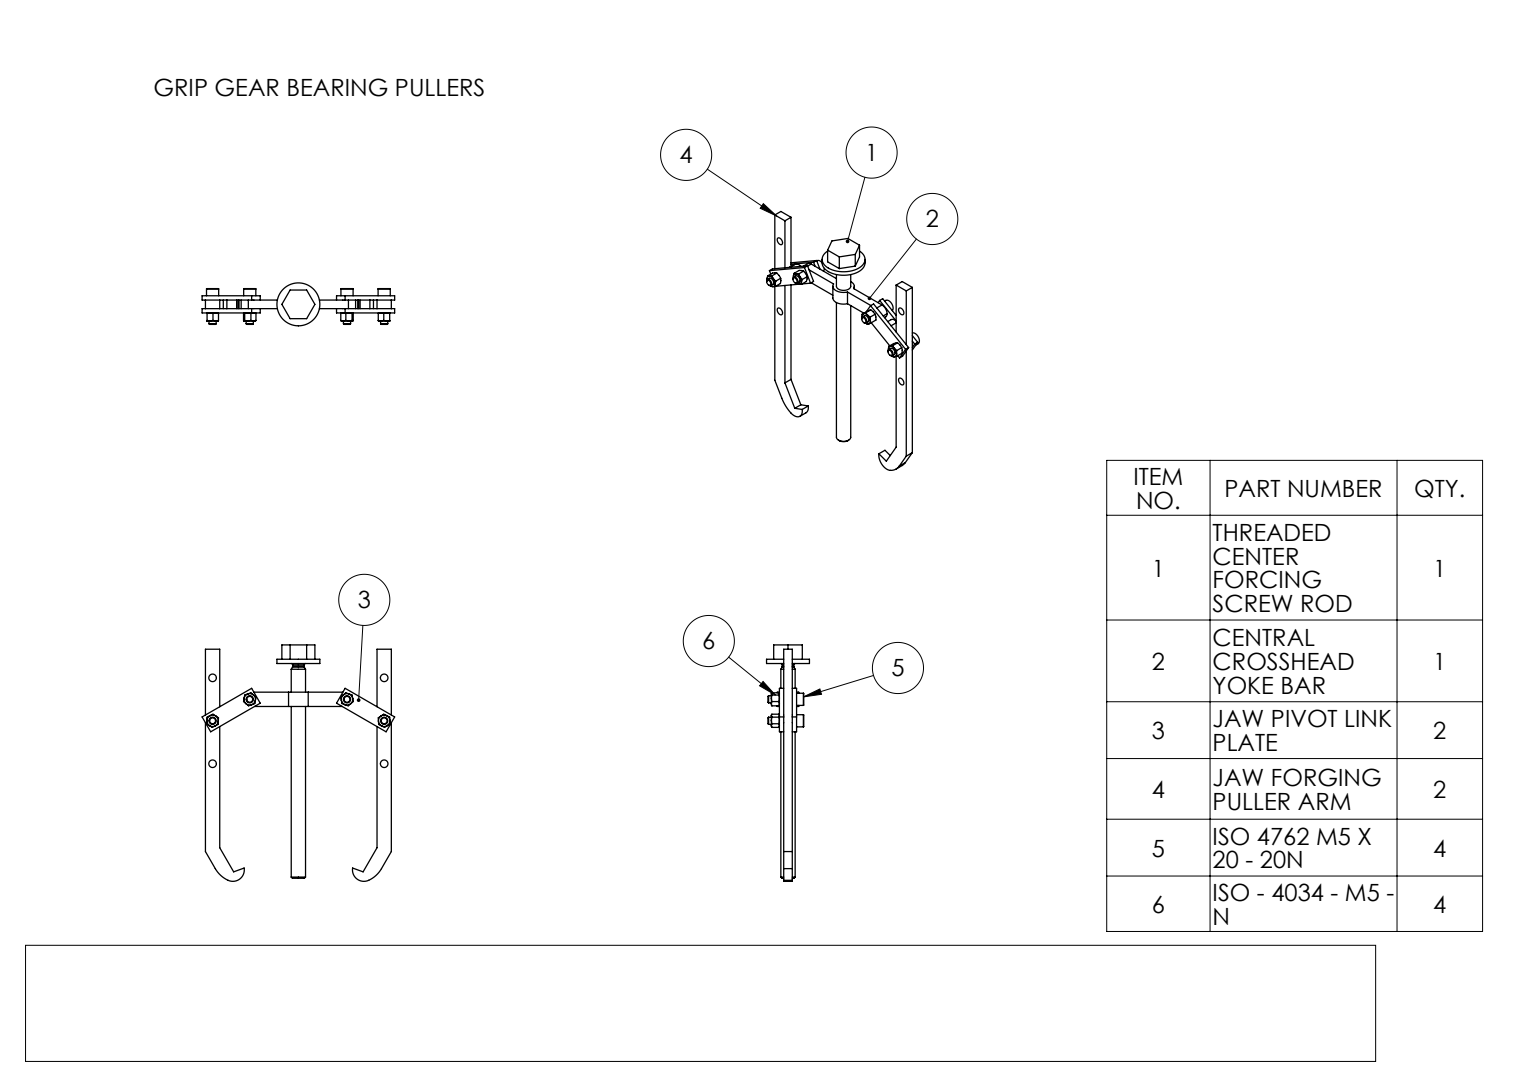
ISO-10303-21;
HEADER;
FILE_DESCRIPTION (('STEP AP214'),
    '1' );
FILE_NAME ('MAS-182',
    '2026-10-22T13:24:12',
    ( '' ),
    ( '' ),
    'SwSTEP 2.0',
    'SolidWorks 2026',
    '' );
FILE_SCHEMA (( 'AUTOMOTIVE_DESIGN' ));
ENDSEC;

DATA;
#1 = DIRECTION ( 'NONE',  ( 1.000000000000000000, 0.000000000000000000, 0.000000000000000000 ) ) ;
#2 = CARTESIAN_POINT ( 'NONE',  ( 0.000000000000000000, -150.0000000000000000, 0.000000000000000000 ) ) ;
#3 = AXIS2_PLACEMENT_3D ( 'NONE', #2223, #202, #1998 ) ;
#4 = EDGE_CURVE ( 'NONE', #2839, #391, #2268, .T. ) ;
#5 = LINE ( 'NONE', #437, #2768 ) ;
#6 = VECTOR ( 'NONE', #2626, 1000.000000000000114 ) ;
#7 = VECTOR ( 'NONE', #1963, 1000.000000000000000 ) ;
#8 = ORIENTED_EDGE ( 'NONE', *, *, #1854, .F. ) ;
#9 = CARTESIAN_POINT ( 'NONE',  ( -18.00961894323348389, -42.69615242270662492, -3.000000000000000000 ) ) ;
#10 = PLANE ( 'NONE',  #689 ) ;
#11 = AXIS2_PLACEMENT_3D ( 'NONE', #480, #2053, #1136 ) ;
#12 = CARTESIAN_POINT ( 'NONE',  ( 5.510910596163087583E-16, -0.9999999999999997780, -3.999999999999999112 ) ) ;
#13 = COLOUR_RGB ( '',0.8941176470588234615, 0.8941176470588234615, 0.8941176470588234615 ) ;
#14 = DIRECTION ( 'NONE',  ( -1.000000000000000000, 0.000000000000000000, 1.502314598737159524E-16 ) ) ;
#15 = VERTEX_POINT ( 'NONE', #913 ) ;
#16 = DIRECTION ( 'NONE',  ( 0.000000000000000000, 0.000000000000000000, -1.000000000000000000 ) ) ;
#17 = DIRECTION ( 'NONE',  ( -1.000000000000000000, 0.000000000000000000, 3.004629197474320528E-16 ) ) ;
#18 = DIRECTION ( 'NONE',  ( -0.000000000000000000, -1.000000000000000000, -0.000000000000000000 ) ) ;
#19 = VECTOR ( 'NONE', #1794, 1000.000000000000000 ) ;
#20 = PRODUCT_DEFINITION_SHAPE ( 'NONE', 'NONE',  #1387 ) ;
#21 = EDGE_CURVE ( 'NONE', #1828, #1252, #472, .T. ) ;
#22 = VECTOR ( 'NONE', #2319, 1000.000000000000000 ) ;
#23 = VERTEX_POINT ( 'NONE', #2540 ) ;
#24 = DIRECTION ( 'NONE',  ( 0.000000000000000000, 0.7071067811865452413, 0.7071067811865497932 ) ) ;
#25 = FACE_OUTER_BOUND ( 'NONE', #1470, .T. ) ;
#26 = VERTEX_POINT ( 'NONE', #2286 ) ;
#27 = CARTESIAN_POINT ( 'NONE',  ( -5.773502691896258199, 13.00000000000000178, -9.999999999999998224 ) ) ;
#28 = EDGE_CURVE ( 'NONE', #2653, #1371, #1839, .T. ) ;
#29 = ORIENTED_EDGE ( 'NONE', *, *, #1848, .F. ) ;
#30 = DIRECTION ( 'NONE',  ( -1.000000000000000000, 0.000000000000000000, 0.000000000000000000 ) ) ;
#31 = FACE_OUTER_BOUND ( 'NONE', #195, .T. ) ;
#32 = FACE_OUTER_BOUND ( 'NONE', #973, .T. ) ;
#33 = CARTESIAN_POINT ( 'NONE',  ( -32.66987298107778059, -17.30384757729337508, 6.000000000000000000 ) ) ;
#34 = ORIENTED_EDGE ( 'NONE', *, *, #947, .F. ) ;
#35 = DIRECTION ( 'NONE',  ( 1.000000000000000000, 0.000000000000000000, 0.000000000000000000 ) ) ;
#36 = EDGE_CURVE ( 'NONE', #1503, #53, #2280, .T. ) ;
#37 = CARTESIAN_POINT ( 'NONE',  ( -36.64999999999999147, -25.00000000000000000, 6.000000000000000888 ) ) ;
#38 = ADVANCED_FACE ( 'NONE', ( #500, #1172 ), #2089, .T. ) ;
#39 = DIRECTION ( 'NONE',  ( -1.000000000000000000, 0.000000000000000000, 0.000000000000000000 ) ) ;
#40 = SURFACE_SIDE_STYLE ('',( #2060 ) ) ;
#41 = ORIENTED_EDGE ( 'NONE', *, *, #2625, .F. ) ;
#42 = CARTESIAN_POINT ( 'NONE',  ( -43.16025403784440329, -29.13397459621553764, 3.000000000000002220 ) ) ;
#43 = DIRECTION ( 'NONE',  ( -0.000000000000000000, -1.000000000000000000, -0.000000000000000000 ) ) ;
#44 = DIRECTION ( 'NONE',  ( 0.000000000000000000, 1.000000000000000000, 0.000000000000000000 ) ) ;
#45 = FACE_OUTER_BOUND ( 'NONE', #672, .T. ) ;
#46 = AXIS2_PLACEMENT_3D ( 'NONE', #1452, #789, #2135 ) ;
#47 = EDGE_LOOP ( 'NONE', ( #341, #1054, #52, #1581 ) ) ;
#48 = CARTESIAN_POINT ( 'NONE',  ( -34.99999999999999289, -20.00000000000000000, 3.000000000000000000 ) ) ;
#49 = CIRCLE ( 'NONE', #831, 7.500000000000000888 ) ;
#50 = FACE_BOUND ( 'NONE', #2831, .T. ) ;
#51 = AXIS2_PLACEMENT_3D ( 'NONE', #933, #1833, #2774 ) ;
#52 = ORIENTED_EDGE ( 'NONE', *, *, #1034, .T. ) ;
#53 = VERTEX_POINT ( 'NONE', #12 ) ;
#54 = AXIS2_PLACEMENT_3D ( 'NONE', #2910, #888, #418 ) ;
#55 = EDGE_CURVE ( 'NONE', #2070, #608, #62, .T. ) ;
#56 = CARTESIAN_POINT ( 'NONE',  ( 0.000000000000000000, -1.000000000000000000, 0.000000000000000000 ) ) ;
#57 = ORIENTED_EDGE ( 'NONE', *, *, #910, .F. ) ;
#58 = AXIS2_PLACEMENT_3D ( 'NONE', #1165, #883, #1343 ) ;
#59 = CARTESIAN_POINT ( 'NONE',  ( -58.09974666316955449, -143.2580143298517328, -3.000000000000000000 ) ) ;
#60 = DIRECTION ( 'NONE',  ( -0.8660254037844401509, -0.4999999999999971689, 1.469576158976821827E-16 ) ) ;
#61 = DIRECTION ( 'NONE',  ( 1.000000000000000000, 0.000000000000000000, 0.000000000000000000 ) ) ;
#62 = CIRCLE ( 'NONE', #204, 20.00000000000000355 ) ;
#63 = AXIS2_PLACEMENT_3D ( 'NONE', #554, #2133, #1693 ) ;
#64 = ORIENTED_EDGE ( 'NONE', *, *, #1925, .F. ) ;
#65 = EDGE_CURVE ( 'NONE', #415, #110, #2593, .T. ) ;
#66 = PLANE ( 'NONE',  #2475 ) ;
#67 = AXIS2_PLACEMENT_3D ( 'NONE', #278, #535, #1657 ) ;
#68 = EDGE_CURVE ( 'NONE', #2151, #2048, #2812, .T. ) ;
#69 = LINE ( 'NONE', #303, #372 ) ;
#70 = ORIENTED_EDGE ( 'NONE', *, *, #879, .F. ) ;
#71 = CIRCLE ( 'NONE', #1705, 4.999999999999998224 ) ;
#72 = CARTESIAN_POINT ( 'NONE',  ( -52.65063509461111835, -62.69615242270656807, -3.000000000000000000 ) ) ;
#73 = CARTESIAN_POINT ( 'NONE',  ( -43.99038105676666532, -37.69615242270662492, 3.000000000000002665 ) ) ;
#74 = ORIENTED_EDGE ( 'NONE', *, *, #1121, .T. ) ;
#75 = EDGE_CURVE ( 'NONE', #120, #1771, #154, .T. ) ;
#76 = CYLINDRICAL_SURFACE ( 'NONE', #302, 2.649999999999985700 ) ;
#77 = FILL_AREA_STYLE_COLOUR ( '', #559 ) ;
#78 = LINE ( 'NONE', #2340, #2456 ) ;
#79 = FACE_BOUND ( 'NONE', #2327, .T. ) ;
#80 = EDGE_CURVE ( 'NONE', #1900, #237, #994, .T. ) ;
#81 = VERTEX_POINT ( 'NONE', #86 ) ;
#82 = LINE ( 'NONE', #1419, #2817 ) ;
#83 = VERTEX_POINT ( 'NONE', #98 ) ;
#84 = CARTESIAN_POINT ( 'NONE',  ( -39.99999999999999289, -30.00000000000000000, -3.000000000000000000 ) ) ;
#85 = ORIENTED_EDGE ( 'NONE', *, *, #1055, .F. ) ;
#86 = CARTESIAN_POINT ( 'NONE',  ( 0.000000000000000000, -149.1719999999999970, 5.000000000000000000 ) ) ;
#87 = CARTESIAN_POINT ( 'NONE',  ( -59.98076211353318854, -39.99999999999994316, 6.000000000000000888 ) ) ;
#88 = ORIENTED_EDGE ( 'NONE', *, *, #2477, .T. ) ;
#89 = LINE ( 'NONE', #2576, #346 ) ;
#90 = DIRECTION ( 'NONE',  ( 0.8660254037844383745, 0.000000000000000000, -0.5000000000000004441 ) ) ;
#91 = DIRECTION ( 'NONE',  ( -0.000000000000000000, -0.000000000000000000, 1.000000000000000000 ) ) ;
#92 = EDGE_CURVE ( 'NONE', #1675, #1139, #1237, .T. ) ;
#93 = VERTEX_POINT ( 'NONE', #2360 ) ;
#94 = AXIS2_PLACEMENT_3D ( 'NONE', #273, #1403, #2068 ) ;
#95 = PLANE ( 'NONE',  #2598 ) ;
#96 = EDGE_LOOP ( 'NONE', ( #402, #361, #2058, #215 ) ) ;
#97=STYLED_ITEM('',(#2949),#2534);
#98 = CARTESIAN_POINT ( 'NONE',  ( -62.63076211353318712, -9.999999999999943157, 3.000000000000001332 ) ) ;
#99 = CARTESIAN_POINT ( 'NONE',  ( -31.35000000000001563, -25.00000000000000000, -3.000000000000001332 ) ) ;
#100 = EDGE_LOOP ( 'NONE', ( #2045, #2281 ) ) ;
#101 = MECHANICAL_DESIGN_GEOMETRIC_PRESENTATION_REPRESENTATION (  '', ( #833 ), #2032 ) ;
#102 = DIRECTION ( 'NONE',  ( -1.000000000000000000, 0.000000000000000000, 0.000000000000000000 ) ) ;
#103 = VECTOR ( 'NONE', #2064, 1000.000000000000114 ) ;
#104 = FILL_AREA_STYLE ('',( #77 ) ) ;
#105 = CARTESIAN_POINT ( 'NONE',  ( -31.00000000000002132, -30.19615242270664268, -3.000000000000000888 ) ) ;
#106 = ADVANCED_FACE ( 'NONE', ( #985 ), #566, .F. ) ;
#107 = VECTOR ( 'NONE', #1157, 1000.000000000000000 ) ;
#108 = ORIENTED_EDGE ( 'NONE', *, *, #1186, .F. ) ;
#109 = CLOSED_SHELL ( 'NONE', ( #2797, #1837, #1415, #550, #392, #827, #441, #1532, #2192, #615, #2313, #2289, #2566, #2325, #660, #1443, #890 ) ) ;
#110 = VERTEX_POINT ( 'NONE', #332 ) ;
#111 = EDGE_CURVE ( 'NONE', #2201, #2834, #2628, .T. ) ;
#112 = VECTOR ( 'NONE', #2880, 1000.000000000000000 ) ;
#113 = EDGE_CURVE ( 'NONE', #132, #2201, #803, .T. ) ;
#114 = LINE ( 'NONE', #1010, #6 ) ;
#115 = EDGE_LOOP ( 'NONE', ( #29, #1418, #842, #2140 ) ) ;
#116 = DIRECTION ( 'NONE',  ( 1.000000000000000000, 0.000000000000000000, 0.000000000000000000 ) ) ;
#117 = AXIS2_PLACEMENT_3D ( 'NONE', #1191, #1902, #2801 ) ;
#118 = DIRECTION ( 'NONE',  ( 0.000000000000000000, 0.000000000000000000, 1.000000000000000000 ) ) ;
#119 = CIRCLE ( 'NONE', #1751, 4.999999999999997335 ) ;
#120 = VERTEX_POINT ( 'NONE', #127 ) ;
#121 = SURFACE_STYLE_USAGE ( .BOTH. , #1056 ) ;
#122 = LINE ( 'NONE', #1519, #2601 ) ;
#123 = ORIENTED_EDGE ( 'NONE', *, *, #92, .F. ) ;
#124 = PRESENTATION_STYLE_ASSIGNMENT (( #2199 ) ) ;
#125 = ORIENTED_EDGE ( 'NONE', *, *, #2038, .F. ) ;
#126 = DIRECTION ( 'NONE',  ( -0.8660254037844390407, 0.000000000000000000, -0.4999999999999993339 ) ) ;
#127 = CARTESIAN_POINT ( 'NONE',  ( -37.91455138073065001, -142.8479302707733041, -3.000000000000000000 ) ) ;
#128 = CARTESIAN_POINT ( 'NONE',  ( -62.63076211353317291, -39.99999999999994316, -3.000000000000005329 ) ) ;
#129 = EDGE_CURVE ( 'NONE', #732, #608, #1011, .T. ) ;
#130 = ORIENTED_EDGE ( 'NONE', *, *, #1665, .T. ) ;
#131 = DIRECTION ( 'NONE',  ( -0.000000000000000000, -0.000000000000000000, 1.000000000000000000 ) ) ;
#132 = VERTEX_POINT ( 'NONE', #1872 ) ;
#133 = DIRECTION ( 'NONE',  ( -2.312964634635742661E-15, 0.000000000000000000, -1.000000000000000000 ) ) ;
#134 =( NAMED_UNIT ( * ) PLANE_ANGLE_UNIT ( ) SI_UNIT ( $, .RADIAN. ) );
#135 = ORIENTED_EDGE ( 'NONE', *, *, #1188, .F. ) ;
#136 = DIRECTION ( 'NONE',  ( 0.000000000000000000, 0.000000000000000000, 1.000000000000000000 ) ) ;
#137 = DIRECTION ( 'NONE',  ( 0.000000000000000000, 0.000000000000000000, 1.000000000000000000 ) ) ;
#138 = SHAPE_DEFINITION_REPRESENTATION ( #683, #470 ) ;
#139 = DIRECTION ( 'NONE',  ( -1.000000000000000000, 0.000000000000000000, 1.272690286469888396E-16 ) ) ;
#140 = EDGE_LOOP ( 'NONE', ( #2113, #808, #665, #2884, #381 ) ) ;
#141 = AXIS2_PLACEMENT_3D ( 'NONE', #801, #2592, #136 ) ;
#142 = EDGE_CURVE ( 'NONE', #1729, #1249, #2519, .T. ) ;
#143 = CARTESIAN_POINT ( 'NONE',  ( -57.33076211353320417, -69.99999999999995737, 3.000000000000001332 ) ) ;
#144 = DIRECTION ( 'NONE',  ( 1.000000000000000000, 0.000000000000000000, -2.341876692568690761E-15 ) ) ;
#145 = TOROIDAL_SURFACE ( 'NONE', #1548, 4.999999999999998224, 0.9999999999999995559 ) ;
#146 = ORIENTED_EDGE ( 'NONE', *, *, #1085, .T. ) ;
#147 = CYLINDRICAL_SURFACE ( 'NONE', #663, 5.000000000000000888 ) ;
#148=STYLED_ITEM('',(#2977),#1527);
#149 = ORIENTED_EDGE ( 'NONE', *, *, #1965, .T. ) ;
#150 = CIRCLE ( 'NONE', #652, 2.649999999999985700 ) ;
#151 = CARTESIAN_POINT ( 'NONE',  ( -31.00000000000002132, -30.19615242270664268, 6.000000000000000000 ) ) ;
#152 = EDGE_CURVE ( 'NONE', #1771, #732, #1431, .T. ) ;
#153 = CYLINDRICAL_SURFACE ( 'NONE', #1179, 3.999999999999998224 ) ;
#154 = CIRCLE ( 'NONE', #1792, 8.000000000000000000 ) ;
#155 = APPLICATION_PROTOCOL_DEFINITION ( 'draft international standard', 'automotive_design', 1998, #2613 ) ;
#156 = CARTESIAN_POINT ( 'NONE',  ( -18.00961894323348389, -42.69615242270662492, 3.000000000000000000 ) ) ;
#157 = EDGE_LOOP ( 'NONE', ( #1667, #2865, #926, #590, #162 ) ) ;
#158 = VECTOR ( 'NONE', #1568, 1000.000000000000000 ) ;
#159 = SURFACE_STYLE_FILL_AREA ( #1906 ) ;
#160 = DIRECTION ( 'NONE',  ( 1.000000000000000000, 0.000000000000000000, 0.000000000000000000 ) ) ;
#161 = ADVANCED_FACE ( 'NONE', ( #1024 ), #786, .F. ) ;
#162 = ORIENTED_EDGE ( 'NONE', *, *, #1048, .T. ) ;
#163 = FACE_OUTER_BOUND ( 'NONE', #394, .T. ) ;
#164 = EDGE_CURVE ( 'NONE', #1727, #2749, #1701, .T. ) ;
#165 = EDGE_LOOP ( 'NONE', ( #896, #1637 ) ) ;
#166 =( NAMED_UNIT ( * ) SI_UNIT ( $, .STERADIAN. ) SOLID_ANGLE_UNIT ( ) );
#167 = VERTEX_POINT ( 'NONE', #2852 ) ;
#168 = DIRECTION ( 'NONE',  ( -0.000000000000000000, -0.000000000000000000, 1.000000000000000000 ) ) ;
#169 = CARTESIAN_POINT ( 'NONE',  ( 0.000000000000000000, 0.000000000000000000, 0.000000000000000000 ) ) ;
#170 = CARTESIAN_POINT ( 'NONE',  ( 34.00000000000000000, -25.00000000000000000, -3.000000000000001332 ) ) ;
#171 = ORIENTED_EDGE ( 'NONE', *, *, #2056, .F. ) ;
#172 = CYLINDRICAL_SURFACE ( 'NONE', #2274, 3.999999999999998224 ) ;
#173 = CARTESIAN_POINT ( 'NONE',  ( -46.49038105676660848, -33.36602540378440551, -2.999999999999996891 ) ) ;
#174 = ORIENTED_EDGE ( 'NONE', *, *, #892, .F. ) ;
#175 = DIRECTION ( 'NONE',  ( 1.000000000000000000, 0.000000000000000000, 0.000000000000000000 ) ) ;
#176 = SHAPE_REPRESENTATION ( 'MAS-182', ( #2707, #1310, #743, #936, #2461 ), #1979 ) ;
#177 = ORIENTED_EDGE ( 'NONE', *, *, #2792, .T. ) ;
#178 = ADVANCED_FACE ( 'NONE', ( #1439 ), #582, .T. ) ;
#179 = CARTESIAN_POINT ( 'NONE',  ( -6.873863542433761076, -20.00000000000000000, 3.000000000000000000 ) ) ;
#180 = CYLINDRICAL_SURFACE ( 'NONE', #659, 2.649999999999985700 ) ;
#181 = ORIENTED_EDGE ( 'NONE', *, *, #773, .F. ) ;
#182 =( NAMED_UNIT ( * ) SI_UNIT ( $, .STERADIAN. ) SOLID_ANGLE_UNIT ( ) );
#183 = FACE_OUTER_BOUND ( 'NONE', #2189, .T. ) ;
#184 = ORIENTED_EDGE ( 'NONE', *, *, #1754, .T. ) ;
#185 = CIRCLE ( 'NONE', #2071, 2.649999999999985700 ) ;
#186 = DIRECTION ( 'NONE',  ( 1.000000000000000000, 0.000000000000000000, 0.000000000000000000 ) ) ;
#187 = DIRECTION ( 'NONE',  ( -0.000000000000000000, -1.000000000000000000, -0.000000000000000000 ) ) ;
#188 = EDGE_LOOP ( 'NONE', ( #1239, #2686, #729, #1617 ) ) ;
#189 = AXIS2_PLACEMENT_3D ( 'NONE', #2895, #2216, #1972 ) ;
#190 = LINE ( 'NONE', #904, #997 ) ;
#191 = EDGE_CURVE ( 'NONE', #790, #1718, #2828, .T. ) ;
#192 = DIRECTION ( 'NONE',  ( -1.076523719386531503E-16, -6.215312591768280423E-17, 1.000000000000000000 ) ) ;
#193 = AXIS2_PLACEMENT_3D ( 'NONE', #1698, #1267, #144 ) ;
#194 = DIRECTION ( 'NONE',  ( 1.000000000000000000, 0.000000000000000000, 0.000000000000000000 ) ) ;
#195 = EDGE_LOOP ( 'NONE', ( #2000, #2767, #2469, #1038, #802, #746 ) ) ;
#196 = COLOUR_RGB ( '',0.8941176470588234615, 0.8941176470588234615, 0.8941176470588234615 ) ;
#197 = VECTOR ( 'NONE', #522, 1000.000000000000000 ) ;
#198 = LINE ( 'NONE', #2410, #1162 ) ;
#199 = EDGE_CURVE ( 'NONE', #2240, #2529, #1039, .T. ) ;
#200 = FACE_OUTER_BOUND ( 'NONE', #1652, .T. ) ;
#201 =( LENGTH_UNIT ( ) NAMED_UNIT ( * ) SI_UNIT ( .MILLI., .METRE. ) );
#202 = DIRECTION ( 'NONE',  ( -0.000000000000000000, -0.000000000000000000, 1.000000000000000000 ) ) ;
#203 = ORIENTED_EDGE ( 'NONE', *, *, #1188, .T. ) ;
#204 = AXIS2_PLACEMENT_3D ( 'NONE', #900, #2724, #531 ) ;
#205 = DIRECTION ( 'NONE',  ( -1.000000000000000000, 0.000000000000000000, 1.636531581110204284E-16 ) ) ;
#206 = AXIS2_PLACEMENT_3D ( 'NONE', #1277, #1543, #609 ) ;
#207 = FILL_AREA_STYLE_COLOUR ( '', #2269 ) ;
#208 = EDGE_LOOP ( 'NONE', ( #779, #2624, #1671, #1565 ) ) ;
#209 = DIRECTION ( 'NONE',  ( 0.000000000000000000, 0.000000000000000000, 1.000000000000000000 ) ) ;
#210 = VECTOR ( 'NONE', #2756, 1000.000000000000000 ) ;
#211 = CARTESIAN_POINT ( 'NONE',  ( -59.98076211353318854, -69.99999999999995737, 3.000000000000000000 ) ) ;
#212 = VECTOR ( 'NONE', #1969, 1000.000000000000000 ) ;
#213 = DIRECTION ( 'NONE',  ( -0.000000000000000000, -0.000000000000000000, -1.000000000000000000 ) ) ;
#214 = LINE ( 'NONE', #690, #2553 ) ;
#215 = ORIENTED_EDGE ( 'NONE', *, *, #2027, .T. ) ;
#216 = CARTESIAN_POINT ( 'NONE',  ( -31.35000000000001563, -25.00000000000000000, -3.000000000000001332 ) ) ;
#217 = DIRECTION ( 'NONE',  ( 0.000000000000000000, -0.000000000000000000, 1.000000000000000000 ) ) ;
#218 = VERTEX_POINT ( 'NONE', #1654 ) ;
#219 = EDGE_CURVE ( 'NONE', #1447, #1073, #1678, .T. ) ;
#220 = PLANE ( 'NONE',  #1032 ) ;
#221 = DIRECTION ( 'NONE',  ( 0.000000000000000000, 0.000000000000000000, -1.000000000000000000 ) ) ;
#222 = EDGE_LOOP ( 'NONE', ( #1224, #1858, #149, #2137 ) ) ;
#223 = DIRECTION ( 'NONE',  ( -1.000000000000000000, 0.000000000000000000, 0.000000000000000000 ) ) ;
#224 = CARTESIAN_POINT ( 'NONE',  ( -59.98076211353319565, -9.999999999999943157, 3.000000000000000000 ) ) ;
#225 = DIRECTION ( 'NONE',  ( -0.4999999999999977796, 0.8660254037844399289, 0.000000000000000000 ) ) ;
#226 = ORIENTED_EDGE ( 'NONE', *, *, #1897, .F. ) ;
#227 = CARTESIAN_POINT ( 'NONE',  ( 0.000000000000000000, -30.00000000000000000, 0.000000000000000000 ) ) ;
#228 = DIRECTION ( 'NONE',  ( -0.000000000000000000, -1.000000000000000000, -0.000000000000000000 ) ) ;
#229 = EDGE_LOOP ( 'NONE', ( #1491, #1391 ) ) ;
#230 = CARTESIAN_POINT ( 'NONE',  ( -64.98076211353318854, 10.00000000000005684, -3.000000000000000000 ) ) ;
#231 = CARTESIAN_POINT ( 'NONE',  ( 0.000000000000000000, 0.000000000000000000, 0.000000000000000000 ) ) ;
#232 = ORIENTED_EDGE ( 'NONE', *, *, #2574, .F. ) ;
#233 = EDGE_CURVE ( 'NONE', #1447, #2315, #1733, .T. ) ;
#234 = CARTESIAN_POINT ( 'NONE',  ( -59.98076211353318854, -39.99999999999994316, 3.000000000000000444 ) ) ;
#235 = DIRECTION ( 'NONE',  ( -1.000000000000000000, 0.000000000000000000, -0.000000000000000000 ) ) ;
#236 = VECTOR ( 'NONE', #2191, 1000.000000000000000 ) ;
#237 = VERTEX_POINT ( 'NONE', #1323 ) ;
#238 = DIRECTION ( 'NONE',  ( -0.000000000000000000, -0.000000000000000000, 1.000000000000000000 ) ) ;
#239 = AXIS2_PLACEMENT_3D ( 'NONE', #267, #1061, #1149 ) ;
#240 = CIRCLE ( 'NONE', #693, 5.000000000000000000 ) ;
#241 = ORIENTED_EDGE ( 'NONE', *, *, #2815, .T. ) ;
#242 = DIRECTION ( 'NONE',  ( -0.000000000000000000, -0.000000000000000000, 1.000000000000000000 ) ) ;
#243 = MECHANICAL_DESIGN_GEOMETRIC_PRESENTATION_REPRESENTATION (  '', ( #148 ), #1694 ) ;
#244 = ADVANCED_FACE ( 'NONE', ( #397 ), #1289, .T. ) ;
#245 = DIRECTION ( 'NONE',  ( 0.000000000000000000, 0.000000000000000000, 1.000000000000000000 ) ) ;
#246 = EDGE_CURVE ( 'NONE', #218, #2864, #2203, .T. ) ;
#247 = ORIENTED_EDGE ( 'NONE', *, *, #2110, .T. ) ;
#248 = AXIS2_PLACEMENT_3D ( 'NONE', #1579, #1566, #1962 ) ;
#249 = CARTESIAN_POINT ( 'NONE',  ( -37.80724301738815285, -144.1538470861320604, -3.000000000000000000 ) ) ;
#250 = ORIENTED_EDGE ( 'NONE', *, *, #1132, .T. ) ;
#251 = DIRECTION ( 'NONE',  ( -1.000000000000000000, 0.000000000000000000, 1.272690286469888396E-16 ) ) ;
#252 = CARTESIAN_POINT ( 'NONE',  ( -40.77923858748079766, -133.2580143298517044, -3.000000000000000000 ) ) ;
#253 = CARTESIAN_POINT ( 'NONE',  ( -11.54700538379251107, 13.00000000000000178, 3.469741003519073858E-15 ) ) ;
#254 = VECTOR ( 'NONE', #2412, 1000.000000000000000 ) ;
#255 = PRODUCT_DEFINITION_SHAPE ( 'NONE', 'NONE',  #2935 ) ;
#256 = VECTOR ( 'NONE', #2846, 1000.000000000000000 ) ;
#257 = EDGE_CURVE ( 'NONE', #2834, #1447, #2641, .T. ) ;
#258 = EDGE_LOOP ( 'NONE', ( #2402, #1202, #483, #1037 ) ) ;
#259 = LINE ( 'NONE', #2309, #1324 ) ;
#260 = LINE ( 'NONE', #2310, #780 ) ;
#261 = ORIENTED_EDGE ( 'NONE', *, *, #462, .T. ) ;
#262 = CARTESIAN_POINT ( 'NONE',  ( 0.000000000000000000, 0.000000000000000000, -15.00000000000000178 ) ) ;
#263 = SURFACE_STYLE_USAGE ( .BOTH. , #928 ) ;
#264 = EDGE_LOOP ( 'NONE', ( #1087, #283, #1551, #1453 ) ) ;
#265 = CARTESIAN_POINT ( 'NONE',  ( -5.773502691896248429, 3.000000000000000000, 10.00000000000000178 ) ) ;
#266 =( NAMED_UNIT ( * ) PLANE_ANGLE_UNIT ( ) SI_UNIT ( $, .RADIAN. ) );
#267 = CARTESIAN_POINT ( 'NONE',  ( -34.00000000000000000, -25.00000000000000000, -3.000000000000000000 ) ) ;
#268 = CARTESIAN_POINT ( 'NONE',  ( 5.773502691896260863, 13.00000000000000178, 9.999999999999998224 ) ) ;
#269 = ORIENTED_EDGE ( 'NONE', *, *, #725, .T. ) ;
#270 = CARTESIAN_POINT ( 'NONE',  ( -49.19086283016151384, -146.9521719906813928, 3.000000000000000000 ) ) ;
#271 = ADVANCED_FACE ( 'NONE', ( #1528 ), #592, .T. ) ;
#272 =( REPRESENTATION_RELATIONSHIP ('NONE','NONE', #176, #1689 ) REPRESENTATION_RELATIONSHIP_WITH_TRANSFORMATION ( #698 )SHAPE_REPRESENTATION_RELATIONSHIP( ) );
#273 = CARTESIAN_POINT ( 'NONE',  ( 0.000000000000000000, 0.000000000000000000, -3.000000000000000000 ) ) ;
#274 = ORIENTED_EDGE ( 'NONE', *, *, #2038, .T. ) ;
#275 = ORIENTED_EDGE ( 'NONE', *, *, #574, .T. ) ;
#276 = DIRECTION ( 'NONE',  ( -1.000000000000000000, 0.000000000000000000, 0.000000000000000000 ) ) ;
#277 = ORIENTED_EDGE ( 'NONE', *, *, #2792, .F. ) ;
#278 = CARTESIAN_POINT ( 'NONE',  ( 34.00000000000000000, -25.00000000000000000, -3.000000000000001332 ) ) ;
#279 = DIRECTION ( 'NONE',  ( 0.8660254037844397068, 0.4999999999999981681, 0.000000000000000000 ) ) ;
#280 = ADVANCED_FACE ( 'NONE', ( #1721 ), #153, .T. ) ;
#281 = CARTESIAN_POINT ( 'NONE',  ( -59.98076211353318854, -69.99999999999995737, -3.000000000000005329 ) ) ;
#282 = EDGE_CURVE ( 'NONE', #300, #2070, #409, .T. ) ;
#283 = ORIENTED_EDGE ( 'NONE', *, *, #2016, .F. ) ;
#284 = DIRECTION ( 'NONE',  ( 0.000000000000000000, -0.000000000000000000, 1.000000000000000000 ) ) ;
#285 =( GEOMETRIC_REPRESENTATION_CONTEXT ( 3 ) GLOBAL_UNCERTAINTY_ASSIGNED_CONTEXT ( ( #2051 ) ) GLOBAL_UNIT_ASSIGNED_CONTEXT ( ( #2879, #1600, #166 ) ) REPRESENTATION_CONTEXT ( 'NONE', 'WORKASPACE' ) );
#286 = DIRECTION ( 'NONE',  ( 0.000000000000000000, 0.000000000000000000, 1.000000000000000000 ) ) ;
#287 = CIRCLE ( 'NONE', #2368, 4.999999999999997335 ) ;
#288 = ADVANCED_FACE ( 'NONE', ( #385 ), #180, .F. ) ;
#289 = ORIENTED_EDGE ( 'NONE', *, *, #762, .F. ) ;
#290 = EDGE_LOOP ( 'NONE', ( #622, #1114 ) ) ;
#291 = AXIS2_PLACEMENT_3D ( 'NONE', #2036, #2498, #1316 ) ;
#292 = LINE ( 'NONE', #1175, #703 ) ;
#293 = EDGE_CURVE ( 'NONE', #444, #937, #848, .T. ) ;
#294 = VERTEX_POINT ( 'NONE', #1052 ) ;
#295 = VECTOR ( 'NONE', #821, 1000.000000000000000 ) ;
#296 = CARTESIAN_POINT ( 'NONE',  ( -36.99999999999999289, -19.80384757729336087, 3.000000000000004441 ) ) ;
#297 = CARTESIAN_POINT ( 'NONE',  ( 36.64999999999999147, -25.00000000000000000, -3.000000000000001332 ) ) ;
#298 = DIRECTION ( 'NONE',  ( 0.4999999999999998890, 0.000000000000000000, 0.8660254037844385966 ) ) ;
#299 = AXIS2_PLACEMENT_3D ( 'NONE', #2890, #509, #2101 ) ;
#300 = VERTEX_POINT ( 'NONE', #2011 ) ;
#301 = DIRECTION ( 'NONE',  ( -0.000000000000000000, 1.000000000000000000, -0.000000000000000000 ) ) ;
#302 = AXIS2_PLACEMENT_3D ( 'NONE', #1642, #1876, #2515 ) ;
#303 = CARTESIAN_POINT ( 'NONE',  ( -31.00000000000002132, -30.19615242270664268, 3.000000000000004441 ) ) ;
#304 = ORIENTED_EDGE ( 'NONE', *, *, #2625, .T. ) ;
#305 = EDGE_LOOP ( 'NONE', ( #581, #1424, #2061, #2597 ) ) ;
#306 = CARTESIAN_POINT ( 'NONE',  ( 0.000000000000000000, 0.000000000000000000, 0.000000000000000000 ) ) ;
#307 = ORIENTED_EDGE ( 'NONE', *, *, #364, .F. ) ;
#308 = CARTESIAN_POINT ( 'NONE',  ( -55.65063509461099045, -127.4999999999999432, 3.000000000000000000 ) ) ;
#309 = ADVANCED_FACE ( 'NONE', ( #2460 ), #828, .T. ) ;
#310 = UNCERTAINTY_MEASURE_WITH_UNIT (LENGTH_MEASURE( 1.000000000000000082E-05 ), #2495, 'distance_accuracy_value', 'NONE');
#311 = CARTESIAN_POINT ( 'NONE',  ( -62.63076211353317291, -69.99999999999995737, 3.000000000000000000 ) ) ;
#312 = PLANE ( 'NONE',  #1216 ) ;
#313 = CARTESIAN_POINT ( 'NONE',  ( 0.000000000000000000, -30.00000000000000000, 0.000000000000000000 ) ) ;
#314 = ORIENTED_EDGE ( 'NONE', *, *, #2815, .F. ) ;
#315 = CARTESIAN_POINT ( 'NONE',  ( -57.33076211353320417, -39.99999999999994316, 6.000000000000000000 ) ) ;
#316 = ORIENTED_EDGE ( 'NONE', *, *, #1007, .T. ) ;
#317 = DIRECTION ( 'NONE',  ( -0.000000000000000000, -0.000000000000000000, -1.000000000000000000 ) ) ;
#318 = ADVANCED_FACE ( 'NONE', ( #200 ), #1081, .F. ) ;
#319 = FACE_OUTER_BOUND ( 'NONE', #1943, .T. ) ;
#320 = ORIENTED_EDGE ( 'NONE', *, *, #2703, .T. ) ;
#321 = LINE ( 'NONE', #2557, #1703 ) ;
#322 = DIRECTION ( 'NONE',  ( 0.000000000000000000, -0.000000000000000000, 1.000000000000000000 ) ) ;
#323 = DIRECTION ( 'NONE',  ( 0.000000000000000000, 1.000000000000000000, 0.000000000000000000 ) ) ;
#324 = EDGE_CURVE ( 'NONE', #1945, #2225, #2898, .T. ) ;
#325 = ORIENTED_EDGE ( 'NONE', *, *, #21, .F. ) ;
#326 = APPLICATION_CONTEXT ( 'automotive_design' ) ;
#327 = VERTEX_POINT ( 'NONE', #425 ) ;
#328 = CIRCLE ( 'NONE', #2312, 7.500000000000000888 ) ;
#329 = CARTESIAN_POINT ( 'NONE',  ( 5.773502691896260863, 13.00000000000000178, 9.999999999999998224 ) ) ;
#330 = EDGE_LOOP ( 'NONE', ( #811, #74, #1656, #2066 ) ) ;
#331 = CIRCLE ( 'NONE', #981, 5.000000000000000888 ) ;
#332 = CARTESIAN_POINT ( 'NONE',  ( 6.873863542433761076, -30.00000000000000000, 3.000000000000000000 ) ) ;
#333 = CARTESIAN_POINT ( 'NONE',  ( -59.98076211353318854, -69.99999999999995737, 3.000000000000001332 ) ) ;
#334 = ORIENTED_EDGE ( 'NONE', *, *, #1164, .F. ) ;
#335 = CARTESIAN_POINT ( 'NONE',  ( -34.00000000000000000, -25.00000000000000000, -3.000000000000001332 ) ) ;
#336 = AXIS2_PLACEMENT_3D ( 'NONE', #211, #2698, #2453 ) ;
#337 = LINE ( 'NONE', #1932, #2374 ) ;
#338 = DIRECTION ( 'NONE',  ( -0.000000000000000000, 1.000000000000000000, -0.000000000000000000 ) ) ;
#339 = VERTEX_POINT ( 'NONE', #216 ) ;
#340 =( NAMED_UNIT ( * ) SI_UNIT ( $, .STERADIAN. ) SOLID_ANGLE_UNIT ( ) );
#341 = ORIENTED_EDGE ( 'NONE', *, *, #2493, .T. ) ;
#342 = PRODUCT_DEFINITION ( 'UNKNOWN', '', #694, #2622 ) ;
#343 = AXIS2_PLACEMENT_3D ( 'NONE', #865, #2176, #2444 ) ;
#344 = LINE ( 'NONE', #1910, #1067 ) ;
#345 = CARTESIAN_POINT ( 'NONE',  ( 6.873863542433761076, -30.00000000000000000, 3.000000000000000000 ) ) ;
#346 = VECTOR ( 'NONE', #1178, 1000.000000000000114 ) ;
#347 = DIRECTION ( 'NONE',  ( -0.4999999999999968914, 0.8660254037844404840, 0.000000000000000000 ) ) ;
#348 = VECTOR ( 'NONE', #1776, 1000.000000000000000 ) ;
#349 = VERTEX_POINT ( 'NONE', #1259 ) ;
#350 = CARTESIAN_POINT ( 'NONE',  ( 0.000000000000000000, -2.500000000000000444, 0.000000000000000000 ) ) ;
#351 = EDGE_LOOP ( 'NONE', ( #2396, #1986, #2575, #2754 ) ) ;
#352 = DIRECTION ( 'NONE',  ( 0.8660254037844379305, 0.5000000000000014433, -0.000000000000000000 ) ) ;
#353 = ORIENTED_EDGE ( 'NONE', *, *, #1711, .F. ) ;
#354 = CARTESIAN_POINT ( 'NONE',  ( 0.000000000000000000, -30.00000000000000000, 0.000000000000000000 ) ) ;
#355 = EDGE_CURVE ( 'NONE', #1675, #790, #1099, .T. ) ;
#356 = DIRECTION ( 'NONE',  ( 1.000000000000000000, 0.000000000000000000, 0.000000000000000000 ) ) ;
#357 = CARTESIAN_POINT ( 'NONE',  ( -42.16025403784441039, -30.86602540378440906, -2.999999999999997780 ) ) ;
#358 = EDGE_LOOP ( 'NONE', ( #85, #2337, #684, #88 ) ) ;
#359 = FILL_AREA_STYLE_COLOUR ( '', #13 ) ;
#360 = FACE_OUTER_BOUND ( 'NONE', #424, .T. ) ;
#361 = ORIENTED_EDGE ( 'NONE', *, *, #1809, .F. ) ;
#362 = CARTESIAN_POINT ( 'NONE',  ( -34.00000000000000000, -25.00000000000000000, -3.000000000000001332 ) ) ;
#363 = FILL_AREA_STYLE_COLOUR ( '', #196 ) ;
#364 = EDGE_CURVE ( 'NONE', #2326, #862, #2184, .T. ) ;
#365 = ORIENTED_EDGE ( 'NONE', *, *, #2096, .T. ) ;
#366 = EDGE_CURVE ( 'NONE', #1139, #1718, #369, .T. ) ;
#367 = DIRECTION ( 'NONE',  ( -0.000000000000000000, -0.000000000000000000, -1.000000000000000000 ) ) ;
#368 = ORIENTED_EDGE ( 'NONE', *, *, #2549, .T. ) ;
#369 = LINE ( 'NONE', #817, #2570 ) ;
#370 = ADVANCED_FACE ( 'NONE', ( #2055, #484 ), #680, .T. ) ;
#371 = DIRECTION ( 'NONE',  ( -0.000000000000000000, -0.000000000000000000, 1.000000000000000000 ) ) ;
#372 = VECTOR ( 'NONE', #1589, 1000.000000000000114 ) ;
#373 = EDGE_LOOP ( 'NONE', ( #515, #1717, #2590, #1913 ) ) ;
#374 = VECTOR ( 'NONE', #2202, 1000.000000000000000 ) ;
#375 = EDGE_CURVE ( 'NONE', #957, #1371, #1659, .T. ) ;
#376 = DIRECTION ( 'NONE',  ( -0.4999999999999981681, 0.8660254037844397068, -0.000000000000000000 ) ) ;
#377 = CIRCLE ( 'NONE', #602, 7.500000000000000888 ) ;
#378 = ORIENTED_EDGE ( 'NONE', *, *, #113, .F. ) ;
#379 = DIRECTION ( 'NONE',  ( -0.000000000000000000, -0.000000000000000000, 1.000000000000000000 ) ) ;
#380 = VECTOR ( 'NONE', #213, 1000.000000000000000 ) ;
#381 = ORIENTED_EDGE ( 'NONE', *, *, #1328, .F. ) ;
#382 = ORIENTED_EDGE ( 'NONE', *, *, #2069, .F. ) ;
#383 = CIRCLE ( 'NONE', #2037, 2.649999999999992806 ) ;
#384 = CARTESIAN_POINT ( 'NONE',  ( -62.63076211353317291, -69.99999999999995737, 3.000000000000001332 ) ) ;
#385 = FACE_OUTER_BOUND ( 'NONE', #2331, .T. ) ;
#386 = APPLICATION_PROTOCOL_DEFINITION ( 'draft international standard', 'automotive_design', 1998, #1482 ) ;
#387 = CARTESIAN_POINT ( 'NONE',  ( -59.98076211353318854, -69.99999999999995737, 3.000000000000001332 ) ) ;
#388 = VECTOR ( 'NONE', #1937, 1000.000000000000000 ) ;
#389 = ORIENTED_EDGE ( 'NONE', *, *, #2257, .T. ) ;
#390 = CARTESIAN_POINT ( 'NONE',  ( -54.98076211353318143, -128.6602540378443393, 3.000000000000000000 ) ) ;
#391 = VERTEX_POINT ( 'NONE', #1838 ) ;
#392 = ADVANCED_FACE ( 'NONE', ( #2249 ), #1339, .T. ) ;
#393 = DIRECTION ( 'NONE',  ( -0.000000000000000000, -0.000000000000000000, -1.000000000000000000 ) ) ;
#394 = EDGE_LOOP ( 'NONE', ( #2893, #2844, #823, #135 ) ) ;
#395 = CYLINDRICAL_SURFACE ( 'NONE', #239, 2.649999999999992806 ) ;
#396 = ORIENTED_EDGE ( 'NONE', *, *, #1940, .F. ) ;
#397 = FACE_OUTER_BOUND ( 'NONE', #2041, .T. ) ;
#398 = DIRECTION ( 'NONE',  ( 0.4999999999999977796, -0.8660254037844398178, 0.000000000000000000 ) ) ;
#399 = VERTEX_POINT ( 'NONE', #2734 ) ;
#400 = ADVANCED_FACE ( 'NONE', ( #439 ), #66, .T. ) ;
#401 = CARTESIAN_POINT ( 'NONE',  ( -57.33076211353320417, -39.99999999999994316, -3.000000000000005329 ) ) ;
#402 = ORIENTED_EDGE ( 'NONE', *, *, #1276, .T. ) ;
#403 = CARTESIAN_POINT ( 'NONE',  ( -31.35000000000000853, -25.00000000000000000, -3.000000000000000000 ) ) ;
#404 = LINE ( 'NONE', #1296, #697 ) ;
#405 = ADVANCED_FACE ( 'NONE', ( #1352 ), #696, .T. ) ;
#406 = DIRECTION ( 'NONE',  ( 0.000000000000000000, 0.000000000000000000, 1.000000000000000000 ) ) ;
#407 = ORIENTED_EDGE ( 'NONE', *, *, #246, .F. ) ;
#408 = PRODUCT_DEFINITION_SHAPE ( 'NONE', 'NONE',  #2932 ) ;
#409 = LINE ( 'NONE', #626, #254 ) ;
#410 = CYLINDRICAL_SURFACE ( 'NONE', #3, 2.649999999999985700 ) ;
#411 = ORIENTED_EDGE ( 'NONE', *, *, #1925, .T. ) ;
#412 = AXIS2_PLACEMENT_3D ( 'NONE', #1501, #1206, #347 ) ;
#413 = DIRECTION ( 'NONE',  ( -0.000000000000000000, -0.000000000000000000, 1.000000000000000000 ) ) ;
#414 =( NAMED_UNIT ( * ) SI_UNIT ( $, .STERADIAN. ) SOLID_ANGLE_UNIT ( ) );
#415 = VERTEX_POINT ( 'NONE', #2763 ) ;
#416 = AXIS2_PLACEMENT_3D ( 'NONE', #1762, #636, #1319 ) ;
#417 = CARTESIAN_POINT ( 'NONE',  ( -45.80724301738815285, -144.1538470861320604, 3.000000000000000000 ) ) ;
#418 = DIRECTION ( 'NONE',  ( 1.000000000000000000, 0.000000000000000000, 1.636531581110204284E-16 ) ) ;
#419 = VECTOR ( 'NONE', #558, 1000.000000000000000 ) ;
#420 = LINE ( 'NONE', #253, #2911 ) ;
#421 = VECTOR ( 'NONE', #2760, 1000.000000000000227 ) ;
#422 = SURFACE_STYLE_USAGE ( .BOTH. , #1275 ) ;
#423 = CIRCLE ( 'NONE', #2414, 4.171999999999999709 ) ;
#424 = EDGE_LOOP ( 'NONE', ( #674, #785, #2678, #603 ) ) ;
#425 = CARTESIAN_POINT ( 'NONE',  ( 40.00000000000002132, -24.99999999999999645, 3.000000000000000000 ) ) ;
#426 = ADVANCED_FACE ( 'NONE', ( #1140 ), #715, .F. ) ;
#427 = APPLICATION_PROTOCOL_DEFINITION ( 'draft international standard', 'automotive_design', 1998, #2499 ) ;
#428 = CARTESIAN_POINT ( 'NONE',  ( 0.000000000000000000, -2.500000000000000444, 0.000000000000000000 ) ) ;
#429 = ORIENTED_EDGE ( 'NONE', *, *, #1791, .T. ) ;
#430 = DIRECTION ( 'NONE',  ( -0.000000000000000000, -0.000000000000000000, -1.000000000000000000 ) ) ;
#431 =( NAMED_UNIT ( * ) SI_UNIT ( $, .STERADIAN. ) SOLID_ANGLE_UNIT ( ) );
#432 = EDGE_LOOP ( 'NONE', ( #247, #171, #2273, #2867 ) ) ;
#433 = DIRECTION ( 'NONE',  ( -1.076523719386531503E-16, -6.215312591768280423E-17, 1.000000000000000000 ) ) ;
#434 = CIRCLE ( 'NONE', #2909, 8.000000000000000000 ) ;
#435 = CARTESIAN_POINT ( 'NONE',  ( -52.65063509461111835, -62.69615242270656807, 3.000000000000000000 ) ) ;
#436 = VECTOR ( 'NONE', #2543, 1000.000000000000000 ) ;
#437 = CARTESIAN_POINT ( 'NONE',  ( -5.773502691896248429, 13.00000000000000178, 10.00000000000000178 ) ) ;
#438 = ORIENTED_EDGE ( 'NONE', *, *, #488, .T. ) ;
#439 = FACE_OUTER_BOUND ( 'NONE', #687, .T. ) ;
#440 = DIRECTION ( 'NONE',  ( -0.000000000000000000, -0.000000000000000000, 1.000000000000000000 ) ) ;
#441 = ADVANCED_FACE ( 'NONE', ( #2720 ), #2522, .T. ) ;
#442 = ORIENTED_EDGE ( 'NONE', *, *, #787, .T. ) ;
#443 = CARTESIAN_POINT ( 'NONE',  ( -34.99999999999999289, -30.00000000000000000, -3.000000000000000000 ) ) ;
#444 = VERTEX_POINT ( 'NONE', #48 ) ;
#445 = DIRECTION ( 'NONE',  ( -1.000000000000000000, 0.000000000000000000, 0.000000000000000000 ) ) ;
#446 = UNCERTAINTY_MEASURE_WITH_UNIT (LENGTH_MEASURE( 1.000000000000000082E-05 ), #1432, 'distance_accuracy_value', 'NONE');
#447 = CARTESIAN_POINT ( 'NONE',  ( 0.000000000000000000, -2.500000000000000444, 4.133974596215572284 ) ) ;
#448 = LINE ( 'NONE', #1584, #348 ) ;
#449 = ADVANCED_FACE ( 'NONE', ( #1389 ), #497, .T. ) ;
#450 = ORIENTED_EDGE ( 'NONE', *, *, #895, .F. ) ;
#451 = CARTESIAN_POINT ( 'NONE',  ( -39.99999999999999289, -30.00000000000000000, -3.000000000000000000 ) ) ;
#452 = ITEM_DEFINED_TRANSFORMATION ( 'NONE', 'NONE', #743,  #2652 ) ;
#453 = DIRECTION ( 'NONE',  ( -0.000000000000000000, 1.000000000000000000, -0.000000000000000000 ) ) ;
#454 = ORIENTED_EDGE ( 'NONE', *, *, #762, .T. ) ;
#455 = EDGE_LOOP ( 'NONE', ( #513, #2833, #542, #1258 ) ) ;
#456 = DIRECTION ( 'NONE',  ( -0.000000000000000000, -0.000000000000000000, 1.000000000000000000 ) ) ;
#457 = ADVANCED_FACE ( 'NONE', ( #955 ), #1807, .T. ) ;
#458 = CARTESIAN_POINT ( 'NONE',  ( 0.000000000000000000, -30.00000000000000000, 7.500000000000000888 ) ) ;
#459 = ORIENTED_EDGE ( 'NONE', *, *, #2639, .T. ) ;
#460 = FACE_OUTER_BOUND ( 'NONE', #2218, .T. ) ;
#461 = AXIS2_PLACEMENT_3D ( 'NONE', #84, #2266, #924 ) ;
#462 = EDGE_CURVE ( 'NONE', #349, #2502, #1856, .T. ) ;
#463 = CARTESIAN_POINT ( 'NONE',  ( 0.000000000000000000, 0.000000000000000000, 6.000000000000000000 ) ) ;
#464 = CARTESIAN_POINT ( 'NONE',  ( -36.64999999999999858, -25.00000000000000000, 3.000000000000000000 ) ) ;
#465 =( GEOMETRIC_REPRESENTATION_CONTEXT ( 3 ) GLOBAL_UNCERTAINTY_ASSIGNED_CONTEXT ( ( #646 ) ) GLOBAL_UNIT_ASSIGNED_CONTEXT ( ( #1799, #1594, #1071 ) ) REPRESENTATION_CONTEXT ( 'NONE', 'WORKASPACE' ) );
#466 = COLOUR_RGB ( '',0.8941176470588234615, 0.8941176470588234615, 0.8941176470588234615 ) ;
#467 = ORIENTED_EDGE ( 'NONE', *, *, #2602, .T. ) ;
#468 = CARTESIAN_POINT ( 'NONE',  ( 34.00000000000000000, -25.00000000000000000, -3.000000000000000000 ) ) ;
#469 = VECTOR ( 'NONE', #91, 1000.000000000000000 ) ;
#470 = SHAPE_REPRESENTATION ( 'Jaw Pivot Link Plate', ( #2652 ), #836 ) ;
#471 = CARTESIAN_POINT ( 'NONE',  ( -51.82050807568884210, -34.13397459621553764, -2.999999999999998224 ) ) ;
#472 = LINE ( 'NONE', #1376, #1933 ) ;
#473 = CYLINDRICAL_SURFACE ( 'NONE', #1427, 2.649999999999985700 ) ;
#474 = PRESENTATION_STYLE_ASSIGNMENT (( #1827 ) ) ;
#475 = AXIS2_PLACEMENT_3D ( 'NONE', #2390, #2583, #2376 ) ;
#476 = VERTEX_POINT ( 'NONE', #669 ) ;
#477 = DIRECTION ( 'NONE',  ( 0.8660254037844398178, 0.4999999999999977796, 1.243062518353660769E-16 ) ) ;
#478 = UNCERTAINTY_MEASURE_WITH_UNIT (LENGTH_MEASURE( 1.000000000000000082E-05 ), #1953, 'distance_accuracy_value', 'NONE');
#479 = EDGE_CURVE ( 'NONE', #1049, #81, #1573, .T. ) ;
#480 = CARTESIAN_POINT ( 'NONE',  ( 5.773502691896257311, 13.00000000000000178, -10.00000000000000000 ) ) ;
#481 = AXIS2_PLACEMENT_3D ( 'NONE', #2908, #16, #445 ) ;
#482 = CIRCLE ( 'NONE', #2858, 4.999999999999997335 ) ;
#483 = ORIENTED_EDGE ( 'NONE', *, *, #1201, .T. ) ;
#484 = FACE_OUTER_BOUND ( 'NONE', #157, .T. ) ;
#485 = CONTEXT_DEPENDENT_SHAPE_REPRESENTATION ( #996, #255 ) ;
#486 = CARTESIAN_POINT ( 'NONE',  ( -59.98076211353318854, -39.99999999999994316, 6.000000000000000888 ) ) ;
#487 = ORIENTED_EDGE ( 'NONE', *, *, #685, .T. ) ;
#488 = EDGE_CURVE ( 'NONE', #876, #399, #2283, .T. ) ;
#489 = DIRECTION ( 'NONE',  ( -0.000000000000000000, -0.000000000000000000, 1.000000000000000000 ) ) ;
#490 = EDGE_CURVE ( 'NONE', #237, #444, #259, .T. ) ;
#491 = EDGE_LOOP ( 'NONE', ( #2013, #70, #820, #269 ) ) ;
#492 = DIRECTION ( 'NONE',  ( 0.000000000000000000, 0.000000000000000000, -1.000000000000000000 ) ) ;
#493 = CARTESIAN_POINT ( 'NONE',  ( -34.00000000000000000, -25.00000000000000000, 3.000000000000000888 ) ) ;
#494 = LINE ( 'NONE', #2776, #516 ) ;
#495 = EDGE_CURVE ( 'NONE', #1073, #120, #1819, .T. ) ;
#496 = ORIENTED_EDGE ( 'NONE', *, *, #667, .T. ) ;
#497 = CYLINDRICAL_SURFACE ( 'NONE', #2520, 7.500000000000000888 ) ;
#498 = CARTESIAN_POINT ( 'NONE',  ( 0.000000000000000000, -30.00000000000000000, 0.000000000000000000 ) ) ;
#499 = ORIENTED_EDGE ( 'NONE', *, *, #1348, .T. ) ;
#500 = FACE_BOUND ( 'NONE', #2907, .T. ) ;
#501 = CARTESIAN_POINT ( 'NONE',  ( -62.63076211353318712, -9.999999999999943157, 3.000000000000000000 ) ) ;
#502 = ORIENTED_EDGE ( 'NONE', *, *, #1423, .F. ) ;
#503 = CARTESIAN_POINT ( 'NONE',  ( -57.33076211353320417, -69.99999999999995737, -3.000000000000005329 ) ) ;
#504 = FACE_OUTER_BOUND ( 'NONE', #726, .T. ) ;
#505 = DIRECTION ( 'NONE',  ( -0.000000000000000000, 1.000000000000000000, -0.000000000000000000 ) ) ;
#506 = CARTESIAN_POINT ( 'NONE',  ( -62.63076211353317291, -39.99999999999994316, 3.000000000000000000 ) ) ;
#507 = VECTOR ( 'NONE', #1679, 1000.000000000000000 ) ;
#508 = ORIENTED_EDGE ( 'NONE', *, *, #725, .F. ) ;
#509 = DIRECTION ( 'NONE',  ( -0.000000000000000000, -1.000000000000000000, -0.000000000000000000 ) ) ;
#510 = AXIS2_PLACEMENT_3D ( 'NONE', #2538, #1421, #1142 ) ;
#511 = CARTESIAN_POINT ( 'NONE',  ( 0.000000000000000000, 0.000000000000000000, 3.000000000000000000 ) ) ;
#512 = CIRCLE ( 'NONE', #889, 5.000000000000000000 ) ;
#513 = ORIENTED_EDGE ( 'NONE', *, *, #488, .F. ) ;
#514 = EDGE_CURVE ( 'NONE', #1931, #1630, #755, .T. ) ;
#515 = ORIENTED_EDGE ( 'NONE', *, *, #2863, .F. ) ;
#516 = VECTOR ( 'NONE', #2323, 1000.000000000000000 ) ;
#517 = DIRECTION ( 'NONE',  ( -0.000000000000000000, 1.000000000000000000, -0.000000000000000000 ) ) ;
#518 = ORIENTED_EDGE ( 'NONE', *, *, #1328, .T. ) ;
#519 = PRESENTATION_LAYER_ASSIGNMENT (  '', '', ( #795 ) ) ;
#520 = DIRECTION ( 'NONE',  ( -1.000000000000000000, -0.000000000000000000, -0.000000000000000000 ) ) ;
#521 = EDGE_CURVE ( 'NONE', #1511, #1818, #1561, .T. ) ;
#522 = DIRECTION ( 'NONE',  ( -0.000000000000000000, -0.000000000000000000, 1.000000000000000000 ) ) ;
#523 = CARTESIAN_POINT ( 'NONE',  ( -49.99038105676663690, -27.30384757729335377, -2.999999999999997335 ) ) ;
#524 = DIRECTION ( 'NONE',  ( 0.4999999999999993339, 0.000000000000000000, -0.8660254037844390407 ) ) ;
#525 = VECTOR ( 'NONE', #1246, 1000.000000000000000 ) ;
#526 = AXIS2_PLACEMENT_3D ( 'NONE', #2675, #2659, #1946 ) ;
#527 = ORIENTED_EDGE ( 'NONE', *, *, #1941, .F. ) ;
#528 = CIRCLE ( 'NONE', #1435, 7.500000000000000888 ) ;
#529 = DIRECTION ( 'NONE',  ( 0.000000000000000000, 1.000000000000000000, 0.000000000000000000 ) ) ;
#530 = ORIENTED_EDGE ( 'NONE', *, *, #2477, .F. ) ;
#531 = DIRECTION ( 'NONE',  ( -1.000000000000000000, 0.000000000000000000, 0.000000000000000000 ) ) ;
#532 = EDGE_CURVE ( 'NONE', #2405, #2811, #1844, .T. ) ;
#533 = CARTESIAN_POINT ( 'NONE',  ( 0.000000000000000000, -20.00000000000000000, 0.000000000000000000 ) ) ;
#534 = ORIENTED_EDGE ( 'NONE', *, *, #1800, .T. ) ;
#535 = DIRECTION ( 'NONE',  ( -0.000000000000000000, -0.000000000000000000, -1.000000000000000000 ) ) ;
#536 = CARTESIAN_POINT ( 'NONE',  ( -64.98076211353318854, 10.00000000000005684, 3.000000000000000000 ) ) ;
#537 = DIRECTION ( 'NONE',  ( 0.000000000000000000, -0.000000000000000000, 1.000000000000000000 ) ) ;
#538 = CARTESIAN_POINT ( 'NONE',  ( -41.49038105676660848, -33.36602540378440551, 3.000000000000002665 ) ) ;
#539 = ORIENTED_EDGE ( 'NONE', *, *, #2505, .F. ) ;
#540 = EDGE_CURVE ( 'NONE', #2636, #730, #82, .T. ) ;
#541 = CARTESIAN_POINT ( 'NONE',  ( 6.123233995736766282E-16, -149.1719999999999970, -5.000000000000000000 ) ) ;
#542 = ORIENTED_EDGE ( 'NONE', *, *, #2401, .T. ) ;
#543 = DIRECTION ( 'NONE',  ( 0.000000000000000000, 1.000000000000000000, 0.000000000000000000 ) ) ;
#544 = CARTESIAN_POINT ( 'NONE',  ( -47.49038105676664401, -31.63397459621555186, 6.000000000000000000 ) ) ;
#545 = ORIENTED_EDGE ( 'NONE', *, *, #92, .T. ) ;
#546 = DIRECTION ( 'NONE',  ( -0.000000000000000000, -0.000000000000000000, 1.000000000000000000 ) ) ;
#547 = FACE_OUTER_BOUND ( 'NONE', #614, .T. ) ;
#548 = FACE_OUTER_BOUND ( 'NONE', #2786, .T. ) ;
#549 = ORIENTED_EDGE ( 'NONE', *, *, #293, .F. ) ;
#550 = ADVANCED_FACE ( 'NONE', ( #589 ), #2548, .T. ) ;
#551 = ORIENTED_EDGE ( 'NONE', *, *, #1102, .F. ) ;
#552 = AXIS2_PLACEMENT_3D ( 'NONE', #87, #927, #972 ) ;
#553 = CARTESIAN_POINT ( 'NONE',  ( -31.00000000000002132, -30.19615242270664268, -6.000000000000000000 ) ) ;
#554 = CARTESIAN_POINT ( 'NONE',  ( -45.80724301738815285, -144.1538470861320604, -3.000000000000000000 ) ) ;
#555 = CARTESIAN_POINT ( 'NONE',  ( 0.000000000000000000, 0.000000000000000000, 3.999999999999998224 ) ) ;
#556 = ORIENTED_EDGE ( 'NONE', *, *, #2594, .T. ) ;
#557 = AXIS2_PLACEMENT_3D ( 'NONE', #1093, #1120, #664 ) ;
#558 = DIRECTION ( 'NONE',  ( -0.000000000000000000, -0.000000000000000000, 1.000000000000000000 ) ) ;
#559 = COLOUR_RGB ( '',0.8941176470588234615, 0.8941176470588234615, 0.8941176470588234615 ) ;
#560 = ORIENTED_EDGE ( 'NONE', *, *, #1193, .F. ) ;
#561 = PLANE ( 'NONE',  #1135 ) ;
#562 = ADVANCED_FACE ( 'NONE', ( #163 ), #147, .T. ) ;
#563 = ORIENTED_EDGE ( 'NONE', *, *, #2156, .F. ) ;
#564 = AXIS2_PLACEMENT_3D ( 'NONE', #270, #2042, #727 ) ;
#565 = CARTESIAN_POINT ( 'NONE',  ( -39.66025403784451697, -55.19615242270660360, 3.000000000000001776 ) ) ;
#566 = PLANE ( 'NONE',  #1377 ) ;
#567 = AXIS2_PLACEMENT_3D ( 'NONE', #2486, #2006, #1758 ) ;
#568 = DIRECTION ( 'NONE',  ( -1.000000000000000000, -0.000000000000000000, -0.000000000000000000 ) ) ;
#569 = AXIS2_PLACEMENT_3D ( 'NONE', #764, #1454, #1672 ) ;
#570 = VERTEX_POINT ( 'NONE', #1716 ) ;
#571 = ADVANCED_FACE ( 'NONE', ( #2328 ), #967, .F. ) ;
#572 = DIRECTION ( 'NONE',  ( -1.076523719386531503E-16, -6.215312591768280423E-17, 1.000000000000000000 ) ) ;
#573 = DIRECTION ( 'NONE',  ( 2.312964634635742661E-15, -0.000000000000000000, 1.000000000000000000 ) ) ;
#574 = EDGE_CURVE ( 'NONE', #218, #2093, #528, .T. ) ;
#575 = ORIENTED_EDGE ( 'NONE', *, *, #2314, .T. ) ;
#576 = DIRECTION ( 'NONE',  ( -0.000000000000000000, -0.000000000000000000, -1.000000000000000000 ) ) ;
#577 = APPLICATION_CONTEXT ( 'automotive_design' ) ;
#578 = EDGE_LOOP ( 'NONE', ( #232, #588 ) ) ;
#579 = EDGE_CURVE ( 'NONE', #2653, #2728, #1992, .T. ) ;
#580 = DIRECTION ( 'NONE',  ( 0.8660254037844402619, 0.4999999999999971689, 0.000000000000000000 ) ) ;
#581 = ORIENTED_EDGE ( 'NONE', *, *, #782, .F. ) ;
#582 = CYLINDRICAL_SURFACE ( 'NONE', #117, 4.999999999999997335 ) ;
#583 = EDGE_CURVE ( 'NONE', #1771, #167, #812, .T. ) ;
#584 = LINE ( 'NONE', #2391, #2700 ) ;
#585 = ORIENTED_EDGE ( 'NONE', *, *, #1155, .T. ) ;
#586 = LINE ( 'NONE', #1489, #295 ) ;
#587 = CARTESIAN_POINT ( 'NONE',  ( -34.00000000000000000, -25.00000000000000000, 6.000000000000000000 ) ) ;
#588 = ORIENTED_EDGE ( 'NONE', *, *, #1702, .F. ) ;
#589 = FACE_OUTER_BOUND ( 'NONE', #1154, .T. ) ;
#590 = ORIENTED_EDGE ( 'NONE', *, *, #1935, .F. ) ;
#591 = CARTESIAN_POINT ( 'NONE',  ( -40.77923858748079766, -133.2580143298517044, 3.000000000000000000 ) ) ;
#592 = CYLINDRICAL_SURFACE ( 'NONE', #206, 5.000000000000000888 ) ;
#593 = AXIS2_PLACEMENT_3D ( 'NONE', #156, #2118, #139 ) ;
#594 = DIRECTION ( 'NONE',  ( 0.000000000000000000, 0.000000000000000000, 1.000000000000000000 ) ) ;
#595 = PLANE ( 'NONE',  #412 ) ;
#596 = CIRCLE ( 'NONE', #2645, 4.999999999999997335 ) ;
#597 = EDGE_CURVE ( 'NONE', #476, #1951, #2616, .T. ) ;
#598 = ORIENTED_EDGE ( 'NONE', *, *, #1904, .T. ) ;
#599 = VECTOR ( 'NONE', #367, 1000.000000000000000 ) ;
#600 = DIRECTION ( 'NONE',  ( 0.8660254037844401509, 0.4999999999999971689, 1.243062518353660769E-16 ) ) ;
#601 = CARTESIAN_POINT ( 'NONE',  ( -62.63076211353317291, -39.99999999999994316, -3.000000000000001332 ) ) ;
#602 = AXIS2_PLACEMENT_3D ( 'NONE', #2789, #44, #1896 ) ;
#603 = ORIENTED_EDGE ( 'NONE', *, *, #1774, .T. ) ;
#604 = DIRECTION ( 'NONE',  ( -1.076523719386531503E-16, -6.215312591768280423E-17, 1.000000000000000000 ) ) ;
#605 = VECTOR ( 'NONE', #600, 1000.000000000000114 ) ;
#606 = EDGE_LOOP ( 'NONE', ( #2745, #2300, #1536, #1449, #625, #2303, #454, #2564, #695 ) ) ;
#607 = EDGE_CURVE ( 'NONE', #1961, #1828, #1899, .T. ) ;
#608 = VERTEX_POINT ( 'NONE', #2604 ) ;
#609 = DIRECTION ( 'NONE',  ( 1.000000000000000000, 0.000000000000000000, 0.000000000000000000 ) ) ;
#610 = CLOSED_SHELL ( 'NONE', ( #2194, #161, #1974, #571, #178, #2160, #106, #400, #2246, #2065, #1736, #2154, #1658, #1402, #1315, #699, #2001, #2664, #1386, #38, #2587, #2560, #1195, #1955, #750, #1363, #288, #2829, #1653 ) ) ;
#611 = APPLICATION_PROTOCOL_DEFINITION ( 'draft international standard', 'automotive_design', 1998, #577 ) ;
#612 = CARTESIAN_POINT ( 'NONE',  ( 0.000000000000000000, -2.500000000000000444, 0.000000000000000000 ) ) ;
#613 = AXIS2_PLACEMENT_3D ( 'NONE', #2778, #2490, #1152 ) ;
#614 = EDGE_LOOP ( 'NONE', ( #226, #2248, #1244, #2777 ) ) ;
#615 = ADVANCED_FACE ( 'NONE', ( #1270 ), #561, .F. ) ;
#616 = VECTOR ( 'NONE', #2275, 1000.000000000000000 ) ;
#617 = CARTESIAN_POINT ( 'NONE',  ( -61.31088913245541505, -47.69615242270656807, 6.000000000000000000 ) ) ;
#618 = CARTESIAN_POINT ( 'NONE',  ( 6.873863542433758411, -20.00000000000000000, -3.000000000000000000 ) ) ;
#619 = ORIENTED_EDGE ( 'NONE', *, *, #769, .F. ) ;
#620 = LINE ( 'NONE', #1802, #616 ) ;
#621 = CARTESIAN_POINT ( 'NONE',  ( -31.35000000000001563, -25.00000000000000000, 6.000000000000000000 ) ) ;
#622 = ORIENTED_EDGE ( 'NONE', *, *, #1348, .F. ) ;
#623 = DIRECTION ( 'NONE',  ( -1.000000000000000000, 0.000000000000000000, 0.000000000000000000 ) ) ;
#624 = EDGE_CURVE ( 'NONE', #2567, #942, #2819, .T. ) ;
#625 = ORIENTED_EDGE ( 'NONE', *, *, #1622, .F. ) ;
#626 = CARTESIAN_POINT ( 'NONE',  ( -64.31088913245535821, -132.4999999999999432, 3.000000000000000000 ) ) ;
#627 = DIRECTION ( 'NONE',  ( 1.000000000000000000, 0.000000000000000000, 0.000000000000000000 ) ) ;
#628 = CARTESIAN_POINT ( 'NONE',  ( -36.99999999999999289, -19.80384757729336087, 6.000000000000000000 ) ) ;
#629 = ORIENTED_EDGE ( 'NONE', *, *, #2417, .T. ) ;
#630 = DIRECTION ( 'NONE',  ( 0.000000000000000000, 1.000000000000000000, 0.000000000000000000 ) ) ;
#631 = EDGE_LOOP ( 'NONE', ( #499, #763, #2072, #2015 ) ) ;
#632 = FACE_BOUND ( 'NONE', #1715, .T. ) ;
#633 = DIRECTION ( 'NONE',  ( 1.000000000000000000, 0.000000000000000000, 0.000000000000000000 ) ) ;
#634 = EDGE_CURVE ( 'NONE', #2529, #2240, #2044, .T. ) ;
#635 = CYLINDRICAL_SURFACE ( 'NONE', #1883, 4.999999999999997335 ) ;
#636 = DIRECTION ( 'NONE',  ( -0.000000000000000000, -0.000000000000000000, 1.000000000000000000 ) ) ;
#637 = ORIENTED_EDGE ( 'NONE', *, *, #2069, .T. ) ;
#638 = DIRECTION ( 'NONE',  ( -0.000000000000000000, -0.000000000000000000, -1.000000000000000000 ) ) ;
#639 = DIRECTION ( 'NONE',  ( 0.000000000000000000, 1.000000000000000000, 0.000000000000000000 ) ) ;
#640 = VERTEX_POINT ( 'NONE', #1919 ) ;
#641 = VECTOR ( 'NONE', #1326, 1000.000000000000000 ) ;
#642 = DIRECTION ( 'NONE',  ( 1.000000000000000000, 0.000000000000000000, 0.000000000000000000 ) ) ;
#643 = ORIENTED_EDGE ( 'NONE', *, *, #2783, .T. ) ;
#644 = AXIS2_PLACEMENT_3D ( 'NONE', #2442, #863, #2458 ) ;
#645 = DIRECTION ( 'NONE',  ( -0.000000000000000000, -0.000000000000000000, 1.000000000000000000 ) ) ;
#646 = UNCERTAINTY_MEASURE_WITH_UNIT (LENGTH_MEASURE( 1.000000000000000082E-05 ), #1799, 'distance_accuracy_value', 'NONE');
#647 = FACE_OUTER_BOUND ( 'NONE', #1861, .T. ) ;
#648 = CIRCLE ( 'NONE', #1973, 2.649999999999992806 ) ;
#649 = CARTESIAN_POINT ( 'NONE',  ( -46.49038105676660848, -33.36602540378440551, 3.000000000000002220 ) ) ;
#650 = AXIS2_PLACEMENT_3D ( 'NONE', #975, #1444, #1863 ) ;
#651 = EDGE_CURVE ( 'NONE', #2441, #2627, #2183, .T. ) ;
#652 = AXIS2_PLACEMENT_3D ( 'NONE', #1004, #572, #1030 ) ;
#653 = ORIENTED_EDGE ( 'NONE', *, *, #752, .F. ) ;
#654 = DIRECTION ( 'NONE',  ( -0.000000000000000000, -0.000000000000000000, 1.000000000000000000 ) ) ;
#655 = CARTESIAN_POINT ( 'NONE',  ( 0.000000000000000000, -30.00000000000000000, 0.000000000000000000 ) ) ;
#656 = ORIENTED_EDGE ( 'NONE', *, *, #1809, .T. ) ;
#657 = ORIENTED_EDGE ( 'NONE', *, *, #706, .F. ) ;
#658 = CARTESIAN_POINT ( 'NONE',  ( 0.000000000000000000, -20.00000000000000000, 0.000000000000000000 ) ) ;
#659 = AXIS2_PLACEMENT_3D ( 'NONE', #1765, #168, #1063 ) ;
#660 = ADVANCED_FACE ( 'NONE', ( #798 ), #1966, .F. ) ;
#661 = EDGE_LOOP ( 'NONE', ( #2878, #368, #429, #1847, #2459 ) ) ;
#662 = LINE ( 'NONE', #403, #158 ) ;
#663 = AXIS2_PLACEMENT_3D ( 'NONE', #1469, #133, #1035 ) ;
#664 = DIRECTION ( 'NONE',  ( -1.000000000000000000, 3.469446951953614189E-15, 0.000000000000000000 ) ) ;
#665 = ORIENTED_EDGE ( 'NONE', *, *, #925, .T. ) ;
#666 = CARTESIAN_POINT ( 'NONE',  ( 40.00000000000000711, -24.99999999999999645, -3.000000000000000000 ) ) ;
#667 = EDGE_CURVE ( 'NONE', #1818, #1252, #1514, .T. ) ;
#668 = ORIENTED_EDGE ( 'NONE', *, *, #651, .F. ) ;
#669 = CARTESIAN_POINT ( 'NONE',  ( -36.64999999999999147, -25.00000000000000000, -3.000000000000001332 ) ) ;
#670 = LINE ( 'NONE', #1066, #641 ) ;
#671 = EDGE_CURVE ( 'NONE', #1818, #2151, #620, .T. ) ;
#672 = EDGE_LOOP ( 'NONE', ( #2930, #1394, #2851, #2536 ) ) ;
#673 = CARTESIAN_POINT ( 'NONE',  ( 0.000000000000000000, 3.000000000000000000, -15.00000000000000178 ) ) ;
#674 = ORIENTED_EDGE ( 'NONE', *, *, #2651, .F. ) ;
#675 = CARTESIAN_POINT ( 'NONE',  ( 5.773502691896260863, 3.000000000000000000, 9.999999999999998224 ) ) ;
#676 = DIRECTION ( 'NONE',  ( -0.000000000000000000, -0.000000000000000000, 1.000000000000000000 ) ) ;
#677 = ORIENTED_EDGE ( 'NONE', *, *, #2343, .T. ) ;
#678 = LINE ( 'NONE', #1122, #2095 ) ;
#679 = EDGE_LOOP ( 'NONE', ( #539, #585, #496, #1836, #2242, #1273, #1936 ) ) ;
#680 = PLANE ( 'NONE',  #2378 ) ;
#681 = CONTEXT_DEPENDENT_SHAPE_REPRESENTATION ( #2580, #2254 ) ;
#682 = FACE_OUTER_BOUND ( 'NONE', #606, .T. ) ;
#683 = PRODUCT_DEFINITION_SHAPE ( 'NONE', 'NONE',  #982 ) ;
#684 = ORIENTED_EDGE ( 'NONE', *, *, #1451, .T. ) ;
#685 = EDGE_CURVE ( 'NONE', #167, #1073, #434, .T. ) ;
#686 = DIRECTION ( 'NONE',  ( -0.000000000000000000, 1.000000000000000000, -0.000000000000000000 ) ) ;
#687 = EDGE_LOOP ( 'NONE', ( #2861, #960, #108, #2263 ) ) ;
#688 = CARTESIAN_POINT ( 'NONE',  ( -64.98076211353318854, 10.00000000000005684, 3.000000000000000000 ) ) ;
#689 = AXIS2_PLACEMENT_3D ( 'NONE', #628, #1053, #1084 ) ;
#690 = CARTESIAN_POINT ( 'NONE',  ( -49.19086283016151384, -146.9521719906813928, -3.000000000000000000 ) ) ;
#691 = VECTOR ( 'NONE', #2610, 1000.000000000000000 ) ;
#692 = CYLINDRICAL_SURFACE ( 'NONE', #2848, 2.649999999999992806 ) ;
#693 = AXIS2_PLACEMENT_3D ( 'NONE', #1251, #2832, #2860 ) ;
#694 = PRODUCT_DEFINITION_FORMATION_WITH_SPECIFIED_SOURCE ( 'ANY', '', #2336, .NOT_KNOWN. ) ;
#695 = ORIENTED_EDGE ( 'NONE', *, *, #1164, .T. ) ;
#696 = PLANE ( 'NONE',  #708 ) ;
#697 = VECTOR ( 'NONE', #2211, 1000.000000000000000 ) ;
#698 = ITEM_DEFINED_TRANSFORMATION ( 'NONE', 'NONE', #1310,  #2652 ) ;
#699 = ADVANCED_FACE ( 'NONE', ( #632, #460 ), #2452, .F. ) ;
#700 = DIRECTION ( 'NONE',  ( 0.000000000000000000, -0.8660254037844267172, -0.5000000000000207612 ) ) ;
#701 = AXIS2_PLACEMENT_3D ( 'NONE', #1280, #1697, #2617 ) ;
#702 = ORIENTED_EDGE ( 'NONE', *, *, #2333, .F. ) ;
#703 = VECTOR ( 'NONE', #1826, 1000.000000000000000 ) ;
#704 = LINE ( 'NONE', #2770, #1369 ) ;
#705 = VERTEX_POINT ( 'NONE', #1582 ) ;
#706 = EDGE_CURVE ( 'NONE', #790, #2206, #873, .T. ) ;
#707 = PLANE ( 'NONE',  #2476 ) ;
#708 = AXIS2_PLACEMENT_3D ( 'NONE', #1588, #2746, #1605 ) ;
#709 = DIRECTION ( 'NONE',  ( 1.224646799147352468E-16, 0.000000000000000000, -1.000000000000000000 ) ) ;
#710 = PLANE ( 'NONE',  #2891 ) ;
#711 = PLANE ( 'NONE',  #2371 ) ;
#712 = CIRCLE ( 'NONE', #1563, 2.649999999999985700 ) ;
#713 = CIRCLE ( 'NONE', #807, 2.649999999999985700 ) ;
#714 = ORIENTED_EDGE ( 'NONE', *, *, #1505, .F. ) ;
#715 = CYLINDRICAL_SURFACE ( 'NONE', #1894, 2.649999999999992806 ) ;
#716 = FACE_BOUND ( 'NONE', #813, .T. ) ;
#717 = EDGE_LOOP ( 'NONE', ( #289, #2875, #2214, #2681 ) ) ;
#718 = EDGE_LOOP ( 'NONE', ( #2082, #993, #8, #549 ) ) ;
#719 = FACE_OUTER_BOUND ( 'NONE', #1079, .T. ) ;
#720 = ORIENTED_EDGE ( 'NONE', *, *, #2117, .F. ) ;
#721 = LINE ( 'NONE', #688, #436 ) ;
#722 = FACE_OUTER_BOUND ( 'NONE', #717, .T. ) ;
#723 = DIRECTION ( 'NONE',  ( 0.000000000000000000, 0.000000000000000000, 1.000000000000000000 ) ) ;
#724 = DIRECTION ( 'NONE',  ( 0.000000000000000000, 0.000000000000000000, -1.000000000000000000 ) ) ;
#725 = EDGE_CURVE ( 'NONE', #2634, #942, #2927, .T. ) ;
#726 = EDGE_LOOP ( 'NONE', ( #2547, #2181, #1068, #1158, #556 ) ) ;
#727 = DIRECTION ( 'NONE',  ( -0.9396926207859063185, -0.3420201433256743195, 0.000000000000000000 ) ) ;
#728 = FACE_BOUND ( 'NONE', #2290, .T. ) ;
#729 = ORIENTED_EDGE ( 'NONE', *, *, #1941, .T. ) ;
#730 = VERTEX_POINT ( 'NONE', #2210 ) ;
#731 = DIRECTION ( 'NONE',  ( -0.000000000000000000, -0.000000000000000000, 1.000000000000000000 ) ) ;
#732 = VERTEX_POINT ( 'NONE', #2497 ) ;
#733 = CARTESIAN_POINT ( 'NONE',  ( -34.99999999999999289, -24.99999999999999645, -3.000000000000000000 ) ) ;
#734 = CARTESIAN_POINT ( 'NONE',  ( 0.000000000000000000, -1.999999999999980016, 0.000000000000000000 ) ) ;
#735 = CARTESIAN_POINT ( 'NONE',  ( 0.000000000000000000, 0.000000000000000000, 0.000000000000000000 ) ) ;
#736 = VECTOR ( 'NONE', #1465, 1000.000000000000000 ) ;
#737 = VERTEX_POINT ( 'NONE', #1314 ) ;
#738 = EDGE_CURVE ( 'NONE', #1558, #23, #1382, .T. ) ;
#739 = LINE ( 'NONE', #315, #1592 ) ;
#740 = CIRCLE ( 'NONE', #2556, 2.649999999999985700 ) ;
#741 = VERTEX_POINT ( 'NONE', #1537 ) ;
#742 = DIRECTION ( 'NONE',  ( 1.000000000000000000, 0.000000000000000000, 0.000000000000000000 ) ) ;
#743 = AXIS2_PLACEMENT_3D ( 'NONE', #1083, #1290, #2899 ) ;
#744 = AXIS2_PLACEMENT_3D ( 'NONE', #1788, #1569, #633 ) ;
#745 = DIRECTION ( 'NONE',  ( -0.000000000000000000, -1.000000000000000000, -0.000000000000000000 ) ) ;
#746 = ORIENTED_EDGE ( 'NONE', *, *, #366, .T. ) ;
#747 = AXIS2_PLACEMENT_3D ( 'NONE', #1383, #1180, #2773 ) ;
#748 = CARTESIAN_POINT ( 'NONE',  ( -62.63076211353317291, -69.99999999999995737, -3.000000000000005329 ) ) ;
#749 = SURFACE_STYLE_FILL_AREA ( #932 ) ;
#750 = ADVANCED_FACE ( 'NONE', ( #1092 ), #2035, .T. ) ;
#751 = CARTESIAN_POINT ( 'NONE',  ( -43.16025403784440329, -29.13397459621553764, -2.999999999999997780 ) ) ;
#752 = EDGE_CURVE ( 'NONE', #2529, #1384, #190, .T. ) ;
#753 = DIRECTION ( 'NONE',  ( -0.000000000000000000, -1.000000000000000000, -0.000000000000000000 ) ) ;
#754 = CLOSED_SHELL ( 'NONE', ( #2881, #457, #2145, #2721, #1585, #2277, #1625, #2040, #2699, #1248, #2372, #1234, #1321, #2735, #2694, #1354, #2112, #1825, #280, #1540, #2775, #309, #1255, #405 ) ) ;
#755 = CIRCLE ( 'NONE', #2422, 2.649999999999985700 ) ;
#756 = EDGE_LOOP ( 'NONE', ( #1133, #2308, #2005, #864 ) ) ;
#757 = AXIS2_PLACEMENT_3D ( 'NONE', #1522, #1553, #251 ) ;
#758 = CARTESIAN_POINT ( 'NONE',  ( -59.98076211353318854, -39.99999999999994316, -3.000000000000000888 ) ) ;
#759 = ORIENTED_EDGE ( 'NONE', *, *, #1412, .F. ) ;
#760 = DIRECTION ( 'NONE',  ( -1.000000000000000000, 0.000000000000000000, 0.000000000000000000 ) ) ;
#761 = FACE_OUTER_BOUND ( 'NONE', #2167, .T. ) ;
#762 = EDGE_CURVE ( 'NONE', #1742, #1508, #2230, .T. ) ;
#763 = ORIENTED_EDGE ( 'NONE', *, *, #2164, .T. ) ;
#764 = CARTESIAN_POINT ( 'NONE',  ( -34.00000000000000000, -25.00000000000000000, 3.000000000000000888 ) ) ;
#765 = CARTESIAN_POINT ( 'NONE',  ( -34.99999999999999289, -24.99999999999999645, 3.000000000000000000 ) ) ;
#766 = VERTEX_POINT ( 'NONE', #675 ) ;
#767 = ORIENTED_EDGE ( 'NONE', *, *, #75, .F. ) ;
#768 = LINE ( 'NONE', #2375, #2747 ) ;
#769 = EDGE_CURVE ( 'NONE', #2627, #2492, #859, .T. ) ;
#770 = DIRECTION ( 'NONE',  ( -0.000000000000000000, -0.000000000000000000, 1.000000000000000000 ) ) ;
#771 = DIRECTION ( 'NONE',  ( -0.4999999999999996114, 0.000000000000000000, 0.8660254037844388186 ) ) ;
#772 = VERTEX_POINT ( 'NONE', #2471 ) ;
#773 = EDGE_CURVE ( 'NONE', #942, #1945, #119, .T. ) ;
#774 = FACE_OUTER_BOUND ( 'NONE', #1288, .T. ) ;
#775 = DIRECTION ( 'NONE',  ( 0.000000000000000000, 0.000000000000000000, 1.000000000000000000 ) ) ;
#776 = VERTEX_POINT ( 'NONE', #2729 ) ;
#777 = CARTESIAN_POINT ( 'NONE',  ( -37.80724301738815285, -144.1538470861320604, 3.000000000000000000 ) ) ;
#778 =( LENGTH_UNIT ( ) NAMED_UNIT ( * ) SI_UNIT ( .MILLI., .METRE. ) );
#779 = ORIENTED_EDGE ( 'NONE', *, *, #671, .F. ) ;
#780 = VECTOR ( 'NONE', #700, 1000.000000000000114 ) ;
#781 = DIRECTION ( 'NONE',  ( -0.4999999999999996114, 0.000000000000000000, 0.8660254037844388186 ) ) ;
#782 = EDGE_CURVE ( 'NONE', #814, #969, #712, .T. ) ;
#783 = EDGE_CURVE ( 'NONE', #1252, #1204, #482, .T. ) ;
#784 = VECTOR ( 'NONE', #2823, 1000.000000000000114 ) ;
#785 = ORIENTED_EDGE ( 'NONE', *, *, #375, .F. ) ;
#786 = CYLINDRICAL_SURFACE ( 'NONE', #2717, 2.649999999999985700 ) ;
#787 = EDGE_CURVE ( 'NONE', #2799, #1951, #662, .T. ) ;
#788 = CIRCLE ( 'NONE', #1596, 2.649999999999985700 ) ;
#789 = DIRECTION ( 'NONE',  ( -0.000000000000000000, 1.000000000000000000, -0.000000000000000000 ) ) ;
#790 = VERTEX_POINT ( 'NONE', #2256 ) ;
#791 =( GEOMETRIC_REPRESENTATION_CONTEXT ( 3 ) GLOBAL_UNCERTAINTY_ASSIGNED_CONTEXT ( ( #1365 ) ) GLOBAL_UNIT_ASSIGNED_CONTEXT ( ( #1254, #2877, #2606 ) ) REPRESENTATION_CONTEXT ( 'NONE', 'WORKASPACE' ) );
#792 = AXIS2_PLACEMENT_3D ( 'NONE', #224, #2741, #1523 ) ;
#793 = DIRECTION ( 'NONE',  ( -0.000000000000000000, 1.000000000000000000, -0.000000000000000000 ) ) ;
#794 = FACE_OUTER_BOUND ( 'NONE', #1190, .T. ) ;
#795=STYLED_ITEM('',(#2956),#1538);
#796 = EDGE_CURVE ( 'NONE', #444, #2492, #1743, .T. ) ;
#797 = ORIENTED_EDGE ( 'NONE', *, *, #583, .F. ) ;
#798 = FACE_OUTER_BOUND ( 'NONE', #1917, .T. ) ;
#799 = EDGE_CURVE ( 'NONE', #2318, #570, #1086, .T. ) ;
#800 = ORIENTED_EDGE ( 'NONE', *, *, #1284, .T. ) ;
#801 = CARTESIAN_POINT ( 'NONE',  ( 0.000000000000000000, 0.000000000000000000, 0.000000000000000000 ) ) ;
#802 = ORIENTED_EDGE ( 'NONE', *, *, #2239, .F. ) ;
#803 = LINE ( 'NONE', #1707, #1373 ) ;
#804 = VECTOR ( 'NONE', #946, 1000.000000000000000 ) ;
#805 = PRODUCT_CONTEXT ( 'NONE', #2499, 'mechanical' ) ;
#806 = CYLINDRICAL_SURFACE ( 'NONE', #1212, 15.00000000000000178 ) ;
#807 = AXIS2_PLACEMENT_3D ( 'NONE', #335, #2364, #102 ) ;
#808 = ORIENTED_EDGE ( 'NONE', *, *, #1598, .F. ) ;
#809 = DIRECTION ( 'NONE',  ( -0.000000000000000000, 1.000000000000000000, -0.000000000000000000 ) ) ;
#810 = FACE_OUTER_BOUND ( 'NONE', #2369, .T. ) ;
#811 = ORIENTED_EDGE ( 'NONE', *, *, #1012, .F. ) ;
#812 = LINE ( 'NONE', #777, #2141 ) ;
#813 = EDGE_LOOP ( 'NONE', ( #800, #1999 ) ) ;
#814 = VERTEX_POINT ( 'NONE', #748 ) ;
#815 = EDGE_CURVE ( 'NONE', #2093, #1704, #1830, .T. ) ;
#816 = CARTESIAN_POINT ( 'NONE',  ( -32.66987298107778770, -17.30384757729337508, -3.000000000000000000 ) ) ;
#817 = CARTESIAN_POINT ( 'NONE',  ( -52.65063509461111835, -62.69615242270656807, 3.000000000000000000 ) ) ;
#818 = CARTESIAN_POINT ( 'NONE',  ( 0.000000000000000000, 0.000000000000000000, 0.000000000000000000 ) ) ;
#819 = CARTESIAN_POINT ( 'NONE',  ( -51.82050807568884210, -34.13397459621553764, 3.000000000000001776 ) ) ;
#820 = ORIENTED_EDGE ( 'NONE', *, *, #2257, .F. ) ;
#821 = DIRECTION ( 'NONE',  ( 0.5000000000000013323, -0.8660254037844379305, 0.000000000000000000 ) ) ;
#822 = DIRECTION ( 'NONE',  ( 1.000000000000000000, 0.000000000000000000, 0.000000000000000000 ) ) ;
#823 = ORIENTED_EDGE ( 'NONE', *, *, #2549, .F. ) ;
#824 = DIRECTION ( 'NONE',  ( 1.272690286469888396E-16, 7.347880794884083251E-17, 1.000000000000000000 ) ) ;
#825 = EDGE_CURVE ( 'NONE', #937, #2441, #905, .T. ) ;
#826 = ORIENTED_EDGE ( 'NONE', *, *, #738, .T. ) ;
#827 = ADVANCED_FACE ( 'NONE', ( #2062 ), #707, .T. ) ;
#828 = CYLINDRICAL_SURFACE ( 'NONE', #2090, 5.000000000000000000 ) ;
#829 = VECTOR ( 'NONE', #2691, 1000.000000000000227 ) ;
#830 = FACE_OUTER_BOUND ( 'NONE', #1229, .T. ) ;
#831 = AXIS2_PLACEMENT_3D ( 'NONE', #1245, #529, #1690 ) ;
#832 = ORIENTED_EDGE ( 'NONE', *, *, #872, .F. ) ;
#833 = STYLED_ITEM ( 'NONE', ( #474 ), #1110 ) ;
#834 = CARTESIAN_POINT ( 'NONE',  ( -67.31088913245538663, -37.30384757729328271, 6.000000000000000000 ) ) ;
#835 = DIRECTION ( 'NONE',  ( 0.000000000000000000, 0.000000000000000000, -1.000000000000000000 ) ) ;
#836 =( GEOMETRIC_REPRESENTATION_CONTEXT ( 3 ) GLOBAL_UNCERTAINTY_ASSIGNED_CONTEXT ( ( #2258 ) ) GLOBAL_UNIT_ASSIGNED_CONTEXT ( ( #2847, #2142, #340 ) ) REPRESENTATION_CONTEXT ( 'NONE', 'WORKASPACE' ) );
#837 = ORIENTED_EDGE ( 'NONE', *, *, #199, .T. ) ;
#838 = CIRCLE ( 'NONE', #1074, 2.649999999999992806 ) ;
#839 = CARTESIAN_POINT ( 'NONE',  ( -39.99999999999999289, -20.00000000000000000, 3.000000000000000000 ) ) ;
#840 = AXIS2_PLACEMENT_3D ( 'NONE', #1949, #2873, #2632 ) ;
#841 =( REPRESENTATION_RELATIONSHIP ('NONE','NONE', #176, #470 ) REPRESENTATION_RELATIONSHIP_WITH_TRANSFORMATION ( #923 )SHAPE_REPRESENTATION_RELATIONSHIP( ) );
#842 = ORIENTED_EDGE ( 'NONE', *, *, #2826, .F. ) ;
#843 = CARTESIAN_POINT ( 'NONE',  ( -62.63076211353317291, -39.99999999999994316, 3.000000000000001332 ) ) ;
#844 = ORIENTED_EDGE ( 'NONE', *, *, #514, .T. ) ;
#845 = SURFACE_STYLE_FILL_AREA ( #1720 ) ;
#846 = AXIS2_PLACEMENT_3D ( 'NONE', #72, #2552, #2029 ) ;
#847 = DIRECTION ( 'NONE',  ( -0.000000000000000000, 1.000000000000000000, -0.000000000000000000 ) ) ;
#848 = CIRCLE ( 'NONE', #526, 5.000000000000000888 ) ;
#849 = DIRECTION ( 'NONE',  ( 0.000000000000000000, 0.000000000000000000, 1.000000000000000000 ) ) ;
#850 = CARTESIAN_POINT ( 'NONE',  ( -26.66987298107781967, -27.69615242270666045, -6.000000000000000000 ) ) ;
#851 = AXIS2_PLACEMENT_3D ( 'NONE', #1018, #379, #1728 ) ;
#852 = EDGE_CURVE ( 'NONE', #1704, #1900, #1232, .T. ) ;
#853 = ORIENTED_EDGE ( 'NONE', *, *, #2493, .F. ) ;
#854 = VECTOR ( 'NONE', #546, 1000.000000000000000 ) ;
#855 = PRODUCT_RELATED_PRODUCT_CATEGORY ( 'part', '', ( #2336 ) ) ;
#856 = CYLINDRICAL_SURFACE ( 'NONE', #248, 2.649999999999985700 ) ;
#857 = LINE ( 'NONE', #1534, #1783 ) ;
#858 = ORIENTED_EDGE ( 'NONE', *, *, #1284, .F. ) ;
#859 = LINE ( 'NONE', #2697, #2233 ) ;
#860 = CYLINDRICAL_SURFACE ( 'NONE', #336, 2.649999999999985700 ) ;
#861 = CARTESIAN_POINT ( 'NONE',  ( 35.00000000000001421, -20.00000000000000000, -8.095376221225103140E-14 ) ) ;
#862 = VERTEX_POINT ( 'NONE', #2094 ) ;
#863 = DIRECTION ( 'NONE',  ( -0.000000000000000000, -1.000000000000000000, -0.000000000000000000 ) ) ;
#864 = ORIENTED_EDGE ( 'NONE', *, *, #1102, .T. ) ;
#865 = CARTESIAN_POINT ( 'NONE',  ( 0.000000000000000000, -30.00000000000000000, 0.000000000000000000 ) ) ;
#866 = SHAPE_DEFINITION_REPRESENTATION ( #20, #1396 ) ;
#867 = CARTESIAN_POINT ( 'NONE',  ( -34.00000000000000000, -25.00000000000000000, 6.000000000000000888 ) ) ;
#868 = ORIENTED_EDGE ( 'NONE', *, *, #796, .F. ) ;
#869 = DIRECTION ( 'NONE',  ( -0.000000000000000000, -0.000000000000000000, -1.000000000000000000 ) ) ;
#870 = DIRECTION ( 'NONE',  ( -1.000000000000000000, 0.000000000000000000, 1.636531581110204284E-16 ) ) ;
#871 = ORIENTED_EDGE ( 'NONE', *, *, #2130, .T. ) ;
#872 = EDGE_CURVE ( 'NONE', #2834, #93, #916, .T. ) ;
#873 = LINE ( 'NONE', #2437, #2718 ) ;
#874 = FACE_OUTER_BOUND ( 'NONE', #1782, .T. ) ;
#875 = LINE ( 'NONE', #1571, #1613 ) ;
#876 = VERTEX_POINT ( 'NONE', #1849 ) ;
#877 = CARTESIAN_POINT ( 'NONE',  ( -61.31088913245541505, -47.69615242270656807, 6.000000000000000000 ) ) ;
#878 = CARTESIAN_POINT ( 'NONE',  ( -61.31088913245541505, -47.69615242270656807, -6.000000000000000000 ) ) ;
#879 = EDGE_CURVE ( 'NONE', #2648, #2567, #1381, .T. ) ;
#880 = ORIENTED_EDGE ( 'NONE', *, *, #1530, .T. ) ;
#881 = EDGE_CURVE ( 'NONE', #327, #1027, #1663, .T. ) ;
#882 = AXIS2_PLACEMENT_3D ( 'NONE', #2250, #639, #217 ) ;
#883 = DIRECTION ( 'NONE',  ( -0.4999999999999978351, 0.8660254037844399289, 0.000000000000000000 ) ) ;
#884 = ORIENTED_EDGE ( 'NONE', *, *, #815, .F. ) ;
#885 = CIRCLE ( 'NONE', #2702, 15.00000000000000178 ) ;
#886 = DIRECTION ( 'NONE',  ( 1.272690286469888396E-16, 7.347880794884083251E-17, 1.000000000000000000 ) ) ;
#887 = PRODUCT_DEFINITION_CONTEXT ( 'detailed design', #2350, 'design' ) ;
#888 = DIRECTION ( 'NONE',  ( -1.076523719386531503E-16, -6.215312591768280423E-17, 1.000000000000000000 ) ) ;
#889 = AXIS2_PLACEMENT_3D ( 'NONE', #2003, #187, #221 ) ;
#890 = ADVANCED_FACE ( 'NONE', ( #2291 ), #76, .F. ) ;
#891 = DIRECTION ( 'NONE',  ( -2.312964634635742661E-15, 0.000000000000000000, -1.000000000000000000 ) ) ;
#892 = EDGE_CURVE ( 'NONE', #1101, #476, #2304, .T. ) ;
#893 = PRESENTATION_LAYER_ASSIGNMENT (  '', '', ( #2222 ) ) ;
#894 = AXIS2_PLACEMENT_3D ( 'NONE', #2, #2007, #2052 ) ;
#895 = EDGE_CURVE ( 'NONE', #772, #2668, #1610, .T. ) ;
#896 = ORIENTED_EDGE ( 'NONE', *, *, #597, .F. ) ;
#897 = DIRECTION ( 'NONE',  ( -1.000000000000000000, 0.000000000000000000, -0.000000000000000000 ) ) ;
#898 = CONTEXT_DEPENDENT_SHAPE_REPRESENTATION ( #272, #408 ) ;
#899 = CARTESIAN_POINT ( 'NONE',  ( -6.873863542433758411, -30.00000000000000000, -3.000000000000000000 ) ) ;
#900 = CARTESIAN_POINT ( 'NONE',  ( -40.77923858748079766, -133.2580143298517044, 3.000000000000000000 ) ) ;
#901 = CARTESIAN_POINT ( 'NONE',  ( -34.00000000000000000, -25.00000000000000000, 3.000000000000000000 ) ) ;
#902 = AXIS2_PLACEMENT_3D ( 'NONE', #2158, #1001, #137 ) ;
#903 = ORIENTED_EDGE ( 'NONE', *, *, #2472, .T. ) ;
#904 = CARTESIAN_POINT ( 'NONE',  ( -57.33076211353321128, -9.999999999999943157, 3.000000000000000000 ) ) ;
#905 = CIRCLE ( 'NONE', #2573, 5.000000000000000888 ) ;
#906 = CARTESIAN_POINT ( 'NONE',  ( -36.64999999999999147, -25.00000000000000000, -3.000000000000000444 ) ) ;
#907 = LINE ( 'NONE', #1297, #2385 ) ;
#908 = VERTEX_POINT ( 'NONE', #59 ) ;
#909 = DIRECTION ( 'NONE',  ( 1.000000000000000000, 1.486905836551548586E-16, -0.000000000000000000 ) ) ;
#910 = EDGE_CURVE ( 'NONE', #2502, #2634, #89, .T. ) ;
#911 = ORIENTED_EDGE ( 'NONE', *, *, #36, .T. ) ;
#912 = DIRECTION ( 'NONE',  ( -1.272690286469888396E-16, -7.347880794884083251E-17, -1.000000000000000000 ) ) ;
#913 = CARTESIAN_POINT ( 'NONE',  ( -67.31088913245542926, -37.30384757729331113, -3.000000000000000000 ) ) ;
#914 = CARTESIAN_POINT ( 'NONE',  ( -36.64999999999999147, -25.00000000000000000, 3.000000000000001332 ) ) ;
#915 = VERTEX_POINT ( 'NONE', #265 ) ;
#916 = LINE ( 'NONE', #1395, #22 ) ;
#917 = PLANE ( 'NONE',  #2411 ) ;
#918 = CARTESIAN_POINT ( 'NONE',  ( -39.66025403784451697, -55.19615242270660360, -2.999999999999998224 ) ) ;
#919 = DIRECTION ( 'NONE',  ( -0.8660254037844387076, 0.000000000000000000, 0.4999999999999999445 ) ) ;
#920 = EDGE_CURVE ( 'NONE', #1023, #26, #321, .T. ) ;
#921 = ORIENTED_EDGE ( 'NONE', *, *, #1009, .T. ) ;
#922 = DIRECTION ( 'NONE',  ( 0.000000000000000000, 1.000000000000000000, 0.000000000000000000 ) ) ;
#923 = ITEM_DEFINED_TRANSFORMATION ( 'NONE', 'NONE', #936,  #2652 ) ;
#924 = DIRECTION ( 'NONE',  ( -1.000000000000000000, 0.000000000000000000, -0.000000000000000000 ) ) ;
#925 = EDGE_CURVE ( 'NONE', #294, #2085, #930, .T. ) ;
#926 = ORIENTED_EDGE ( 'NONE', *, *, #80, .T. ) ;
#927 = DIRECTION ( 'NONE',  ( -0.000000000000000000, -0.000000000000000000, 1.000000000000000000 ) ) ;
#928 = SURFACE_SIDE_STYLE ('',( #1344 ) ) ;
#929 = EDGE_LOOP ( 'NONE', ( #2115, #2050, #1166, #1699 ) ) ;
#930 = LINE ( 'NONE', #1442, #804 ) ;
#931 = AXIS2_PLACEMENT_3D ( 'NONE', #2480, #2883, #398 ) ;
#932 = FILL_AREA_STYLE ('',( #2305 ) ) ;
#933 = CARTESIAN_POINT ( 'NONE',  ( 0.000000000000000000, -1.000000000000000000, 4.999999999999998224 ) ) ;
#934 = CIRCLE ( 'NONE', #141, 4.999999999999998224 ) ;
#935 = CYLINDRICAL_SURFACE ( 'NONE', #1220, 5.000000000000000000 ) ;
#936 = AXIS2_PLACEMENT_3D ( 'NONE', #2204, #594, #1486 ) ;
#937 = VERTEX_POINT ( 'NONE', #974 ) ;
#938 = DIRECTION ( 'NONE',  ( -0.4999999999999981681, 0.8660254037844397068, -0.000000000000000000 ) ) ;
#939 = CIRCLE ( 'NONE', #291, 1.000000000000000000 ) ;
#940 = FACE_OUTER_BOUND ( 'NONE', #1400, .T. ) ;
#941 = AXIS2_PLACEMENT_3D ( 'NONE', #536, #2097, #322 ) ;
#942 = VERTEX_POINT ( 'NONE', #1814 ) ;
#943 = DIRECTION ( 'NONE',  ( -0.000000000000000000, 1.000000000000000000, -0.000000000000000000 ) ) ;
#944 = CARTESIAN_POINT ( 'NONE',  ( -59.98076211353319565, -9.999999999999943157, 3.000000000000000000 ) ) ;
#945 = ORIENTED_EDGE ( 'NONE', *, *, #2401, .F. ) ;
#946 = DIRECTION ( 'NONE',  ( -0.000000000000000000, -0.000000000000000000, -1.000000000000000000 ) ) ;
#947 = EDGE_CURVE ( 'NONE', #23, #2668, #2739, .T. ) ;
#948 = VECTOR ( 'NONE', #1778, 1000.000000000000227 ) ;
#949 = CARTESIAN_POINT ( 'NONE',  ( 0.000000000000000000, -0.9999999999999997780, 3.999999999999999112 ) ) ;
#950 = PLANE ( 'NONE',  #2507 ) ;
#951 = DIRECTION ( 'NONE',  ( 0.000000000000000000, 0.000000000000000000, -1.000000000000000000 ) ) ;
#952 = AXIS2_PLACEMENT_3D ( 'NONE', #733, #492, #30 ) ;
#953 = VECTOR ( 'NONE', #2121, 1000.000000000000000 ) ;
#954 = ORIENTED_EDGE ( 'NONE', *, *, #2516, .F. ) ;
#955 = FACE_OUTER_BOUND ( 'NONE', #1436, .T. ) ;
#956 = FACE_OUTER_BOUND ( 'NONE', #2363, .T. ) ;
#957 = VERTEX_POINT ( 'NONE', #961 ) ;
#958 = DIRECTION ( 'NONE',  ( -0.000000000000000000, -1.000000000000000000, -0.000000000000000000 ) ) ;
#959 = DIRECTION ( 'NONE',  ( -0.000000000000000000, -0.000000000000000000, 1.000000000000000000 ) ) ;
#960 = ORIENTED_EDGE ( 'NONE', *, *, #2505, .T. ) ;
#961 = CARTESIAN_POINT ( 'NONE',  ( 5.062658757011871940E-16, -2.500000000000000444, -4.133974596215572284 ) ) ;
#962 = LINE ( 'NONE', #1832, #2751 ) ;
#963 = CARTESIAN_POINT ( 'NONE',  ( -11.54700538379251107, 13.00000000000000178, 3.469741003519073858E-15 ) ) ;
#964 = EDGE_CURVE ( 'NONE', #132, #300, #721, .T. ) ;
#965 = FACE_BOUND ( 'NONE', #1338, .T. ) ;
#966 = ORIENTED_EDGE ( 'NONE', *, *, #2439, .F. ) ;
#967 = CYLINDRICAL_SURFACE ( 'NONE', #2425, 2.649999999999985700 ) ;
#968 = DIRECTION ( 'NONE',  ( 0.000000000000000000, 0.000000000000000000, -1.000000000000000000 ) ) ;
#969 = VERTEX_POINT ( 'NONE', #503 ) ;
#970 = DIRECTION ( 'NONE',  ( 1.000000000000000000, -1.387778780781446464E-15, 8.673617379884040402E-17 ) ) ;
#971 = EDGE_CURVE ( 'NONE', #1718, #942, #1597, .T. ) ;
#972 = DIRECTION ( 'NONE',  ( 1.000000000000000000, 0.000000000000000000, 0.000000000000000000 ) ) ;
#973 = EDGE_LOOP ( 'NONE', ( #2546, #534, #1117, #2394 ) ) ;
#974 = CARTESIAN_POINT ( 'NONE',  ( -39.99999999999999289, -25.00000000000000000, 3.000000000000000000 ) ) ;
#975 = CARTESIAN_POINT ( 'NONE',  ( -39.99999999999999289, -30.00000000000000000, 3.000000000000000000 ) ) ;
#976 = DIRECTION ( 'NONE',  ( -0.5000000000000004441, 0.000000000000000000, -0.8660254037844383745 ) ) ;
#977 = DIRECTION ( 'NONE',  ( -1.000000000000000000, 0.000000000000000000, -0.000000000000000000 ) ) ;
#978 = CIRCLE ( 'NONE', #46, 3.999999999999999112 ) ;
#979 = CIRCLE ( 'NONE', #1730, 2.649999999999985700 ) ;
#980 = EDGE_LOOP ( 'NONE', ( #1572, #1607, #2719, #2251, #880, #2436 ) ) ;
#981 = AXIS2_PLACEMENT_3D ( 'NONE', #1993, #2687, #1512 ) ;
#982 = PRODUCT_DEFINITION ( 'UNKNOWN', '', #1072, #1803 ) ;
#983 = DIRECTION ( 'NONE',  ( -0.4999999999999993339, 0.000000000000000000, 0.8660254037844390407 ) ) ;
#984 = ORIENTED_EDGE ( 'NONE', *, *, #2380, .T. ) ;
#985 = FACE_OUTER_BOUND ( 'NONE', #2608, .T. ) ;
#986 =( GEOMETRIC_REPRESENTATION_CONTEXT ( 3 ) GLOBAL_UNCERTAINTY_ASSIGNED_CONTEXT ( ( #478 ) ) GLOBAL_UNIT_ASSIGNED_CONTEXT ( ( #1953, #134, #1510 ) ) REPRESENTATION_CONTEXT ( 'NONE', 'WORKASPACE' ) );
#987 = CIRCLE ( 'NONE', #1651, 2.649999999999985700 ) ;
#988 = DIRECTION ( 'NONE',  ( 1.000000000000000000, 0.000000000000000000, 0.000000000000000000 ) ) ;
#989 = ORIENTED_EDGE ( 'NONE', *, *, #2428, .F. ) ;
#990 = LINE ( 'NONE', #2821, #953 ) ;
#991 = SURFACE_SIDE_STYLE ('',( #1148 ) ) ;
#992 = CARTESIAN_POINT ( 'NONE',  ( 0.000000000000000000, -1.999999999999980016, 3.999999999999998224 ) ) ;
#993 = ORIENTED_EDGE ( 'NONE', *, *, #80, .F. ) ;
#994 = CIRCLE ( 'NONE', #475, 4.999999999999997335 ) ;
#995 = ORIENTED_EDGE ( 'NONE', *, *, #583, .T. ) ;
#996 =( REPRESENTATION_RELATIONSHIP ('NONE','NONE', #176, #1396 ) REPRESENTATION_RELATIONSHIP_WITH_TRANSFORMATION ( #1141 )SHAPE_REPRESENTATION_RELATIONSHIP( ) );
#997 = VECTOR ( 'NONE', #2713, 1000.000000000000000 ) ;
#998 = VERTEX_POINT ( 'NONE', #1862 ) ;
#999 = CYLINDRICAL_SURFACE ( 'NONE', #2840, 7.500000000000000888 ) ;
#1000 = EDGE_CURVE ( 'NONE', #1951, #476, #713, .T. ) ;
#1001 = DIRECTION ( 'NONE',  ( -0.000000000000000000, 1.000000000000000000, -0.000000000000000000 ) ) ;
#1002 = FACE_OUTER_BOUND ( 'NONE', #358, .T. ) ;
#1003 = ORIENTED_EDGE ( 'NONE', *, *, #651, .T. ) ;
#1004 = CARTESIAN_POINT ( 'NONE',  ( -59.98076211353318854, -39.99999999999994316, 3.000000000000000444 ) ) ;
#1005 = CARTESIAN_POINT ( 'NONE',  ( 0.000000000000000000, -149.1719999999999970, 0.000000000000000000 ) ) ;
#1006 = ORIENTED_EDGE ( 'NONE', *, *, #1311, .F. ) ;
#1007 = EDGE_CURVE ( 'NONE', #1517, #1797, #1850, .T. ) ;
#1008 = EDGE_LOOP ( 'NONE', ( #1801, #1380, #1747, #1345 ) ) ;
#1009 = EDGE_CURVE ( 'NONE', #969, #1547, #2586, .T. ) ;
#1010 = CARTESIAN_POINT ( 'NONE',  ( -36.99999999999999289, -19.80384757729336087, 3.000000000000000888 ) ) ;
#1011 = LINE ( 'NONE', #1668, #2903 ) ;
#1012 = EDGE_CURVE ( 'NONE', #2433, #2749, #990, .T. ) ;
#1013 = CARTESIAN_POINT ( 'NONE',  ( -64.98076211353316012, -131.3397459621555754, 3.000000000000000000 ) ) ;
#1014 = ORIENTED_EDGE ( 'NONE', *, *, #634, .T. ) ;
#1015 = PRESENTATION_STYLE_ASSIGNMENT (( #121 ) ) ;
#1016 = LINE ( 'NONE', #2166, #7 ) ;
#1017 = ORIENTED_EDGE ( 'NONE', *, *, #1940, .T. ) ;
#1018 = CARTESIAN_POINT ( 'NONE',  ( -59.98076211353319565, -9.999999999999943157, -3.000000000000005329 ) ) ;
#1019 = ORIENTED_EDGE ( 'NONE', *, *, #706, .T. ) ;
#1020 = AXIS2_PLACEMENT_3D ( 'NONE', #1980, #2677, #1529 ) ;
#1021 = LINE ( 'NONE', #553, #2649 ) ;
#1022 = VECTOR ( 'NONE', #1645, 1000.000000000000000 ) ;
#1023 = VERTEX_POINT ( 'NONE', #2245 ) ;
#1024 = FACE_OUTER_BOUND ( 'NONE', #1867, .T. ) ;
#1025 = DIRECTION ( 'NONE',  ( 0.000000000000000000, 0.000000000000000000, 1.000000000000000000 ) ) ;
#1026 = DIRECTION ( 'NONE',  ( 0.000000000000000000, -0.000000000000000000, -1.000000000000000000 ) ) ;
#1027 = VERTEX_POINT ( 'NONE', #2488 ) ;
#1028 = PRODUCT_DEFINITION_FORMATION_WITH_SPECIFIED_SOURCE ( 'ANY', '', #1535, .NOT_KNOWN. ) ;
#1029 = VECTOR ( 'NONE', #2352, 1000.000000000000000 ) ;
#1030 = DIRECTION ( 'NONE',  ( 1.000000000000000000, 0.000000000000000000, 1.636531581110204284E-16 ) ) ;
#1031 = CYLINDRICAL_SURFACE ( 'NONE', #193, 4.999999999999997335 ) ;
#1032 = AXIS2_PLACEMENT_3D ( 'NONE', #658, #630, #2207 ) ;
#1033 = ORIENTED_EDGE ( 'NONE', *, *, #1228, .F. ) ;
#1034 = EDGE_CURVE ( 'NONE', #2085, #1023, #2261, .T. ) ;
#1035 = DIRECTION ( 'NONE',  ( -1.000000000000000000, 0.000000000000000000, 2.312964634635741478E-15 ) ) ;
#1036 = UNCERTAINTY_MEASURE_WITH_UNIT (LENGTH_MEASURE( 1.000000000000000082E-05 ), #201, 'distance_accuracy_value', 'NONE');
#1037 = ORIENTED_EDGE ( 'NONE', *, *, #2918, .T. ) ;
#1038 = ORIENTED_EDGE ( 'NONE', *, *, #521, .T. ) ;
#1039 = CIRCLE ( 'NONE', #1230, 2.649999999999985700 ) ;
#1040 = CARTESIAN_POINT ( 'NONE',  ( 0.000000000000000000, 0.000000000000000000, 0.000000000000000000 ) ) ;
#1041 = DIRECTION ( 'NONE',  ( -1.000000000000000000, 0.000000000000000000, 0.000000000000000000 ) ) ;
#1042 = DIRECTION ( 'NONE',  ( -0.000000000000000000, -0.000000000000000000, 1.000000000000000000 ) ) ;
#1043 = VERTEX_POINT ( 'NONE', #666 ) ;
#1044 = FACE_OUTER_BOUND ( 'NONE', #1542, .T. ) ;
#1045 = CARTESIAN_POINT ( 'NONE',  ( 11.54700538379251107, 13.00000000000000178, -6.939586148520149327E-15 ) ) ;
#1046 = ORIENTED_EDGE ( 'NONE', *, *, #490, .T. ) ;
#1047 = DIRECTION ( 'NONE',  ( -1.000000000000000000, 1.387778780781446464E-15, 8.673617379884040402E-17 ) ) ;
#1048 = EDGE_CURVE ( 'NONE', #2373, #2093, #448, .T. ) ;
#1049 = VERTEX_POINT ( 'NONE', #1350 ) ;
#1050 = DIRECTION ( 'NONE',  ( -0.4999999999999981681, 0.8660254037844397068, -0.000000000000000000 ) ) ;
#1051 = ORIENTED_EDGE ( 'NONE', *, *, #1375, .T. ) ;
#1052 = CARTESIAN_POINT ( 'NONE',  ( -61.31088913245547189, -47.69615242270656807, -3.000000000000000000 ) ) ;
#1053 = DIRECTION ( 'NONE',  ( -0.4999999999999978351, 0.8660254037844399289, 0.000000000000000000 ) ) ;
#1054 = ORIENTED_EDGE ( 'NONE', *, *, #2457, .F. ) ;
#1055 = EDGE_CURVE ( 'NONE', #1249, #1871, #1541, .T. ) ;
#1056 = SURFACE_SIDE_STYLE ('',( #159 ) ) ;
#1057 = DIRECTION ( 'NONE',  ( -1.272690286469888396E-16, -7.347880794884083251E-17, -1.000000000000000000 ) ) ;
#1058 = VERTEX_POINT ( 'NONE', #843 ) ;
#1059 = DIRECTION ( 'NONE',  ( 0.000000000000000000, 0.000000000000000000, 1.000000000000000000 ) ) ;
#1060 = EDGE_LOOP ( 'NONE', ( #2209, #1680, #1329, #656 ) ) ;
#1061 = DIRECTION ( 'NONE',  ( -0.000000000000000000, -0.000000000000000000, -1.000000000000000000 ) ) ;
#1062 = ORIENTED_EDGE ( 'NONE', *, *, #1866, .T. ) ;
#1063 = DIRECTION ( 'NONE',  ( 1.000000000000000000, 0.000000000000000000, 0.000000000000000000 ) ) ;
#1064 = VECTOR ( 'NONE', #568, 1000.000000000000000 ) ;
#1065 = EDGE_CURVE ( 'NONE', #1905, #776, #420, .T. ) ;
#1066 = CARTESIAN_POINT ( 'NONE',  ( 6.123233995736766282E-16, -149.1719999999999970, -5.000000000000000000 ) ) ;
#1067 = VECTOR ( 'NONE', #2157, 1000.000000000000000 ) ;
#1068 = ORIENTED_EDGE ( 'NONE', *, *, #1521, .F. ) ;
#1069 = CONICAL_SURFACE ( 'NONE', #1688, 5.000000000000000000, 0.7853981633974514986 ) ;
#1070 = DIRECTION ( 'NONE',  ( -0.000000000000000000, -1.000000000000000000, -0.000000000000000000 ) ) ;
#1071 =( NAMED_UNIT ( * ) SI_UNIT ( $, .STERADIAN. ) SOLID_ANGLE_UNIT ( ) );
#1072 = PRODUCT_DEFINITION_FORMATION_WITH_SPECIFIED_SOURCE ( 'ANY', '', #1586, .NOT_KNOWN. ) ;
#1073 = VERTEX_POINT ( 'NONE', #2213 ) ;
#1074 = AXIS2_PLACEMENT_3D ( 'NONE', #2545, #1446, #61 ) ;
#1075 = DIRECTION ( 'NONE',  ( 1.000000000000000000, 0.000000000000000000, 0.000000000000000000 ) ) ;
#1076 = FACE_BOUND ( 'NONE', #2478, .T. ) ;
#1077 = MECHANICAL_DESIGN_GEOMETRIC_PRESENTATION_REPRESENTATION (  '', ( #795 ), #1983 ) ;
#1078 = CARTESIAN_POINT ( 'NONE',  ( 0.000000000000000000, -149.1719999999999970, 0.000000000000000000 ) ) ;
#1079 = EDGE_LOOP ( 'NONE', ( #2132, #1062, #575, #653 ) ) ;
#1080 = EDGE_LOOP ( 'NONE', ( #1185, #1761, #1889, #1111 ) ) ;
#1081 = CYLINDRICAL_SURFACE ( 'NONE', #2136, 2.649999999999992806 ) ;
#1082 = AXIS2_PLACEMENT_3D ( 'NONE', #1112, #909, #2264 ) ;
#1083 = CARTESIAN_POINT ( 'NONE',  ( 0.000000000000000000, 0.000000000000000000, 0.000000000000000000 ) ) ;
#1084 = DIRECTION ( 'NONE',  ( -0.8660254037844398178, -0.4999999999999977796, 0.000000000000000000 ) ) ;
#1085 = EDGE_CURVE ( 'NONE', #1775, #2357, #1996, .T. ) ;
#1086 = CIRCLE ( 'NONE', #1796, 2.649999999999985700 ) ;
#1087 = ORIENTED_EDGE ( 'NONE', *, *, #852, .F. ) ;
#1088 = CIRCLE ( 'NONE', #2620, 5.000000000000000000 ) ;
#1089 = PLANE ( 'NONE',  #2129 ) ;
#1090 = SURFACE_STYLE_USAGE ( .BOTH. , #2467 ) ;
#1091 = ORIENTED_EDGE ( 'NONE', *, *, #55, .T. ) ;
#1092 = FACE_OUTER_BOUND ( 'NONE', #491, .T. ) ;
#1093 = CARTESIAN_POINT ( 'NONE',  ( -45.80724301738815285, -144.1538470861320604, 3.000000000000000000 ) ) ;
#1094 = DIRECTION ( 'NONE',  ( -0.000000000000000000, 1.000000000000000000, -0.000000000000000000 ) ) ;
#1095 = EDGE_CURVE ( 'NONE', #1204, #2567, #678, .T. ) ;
#1096 = DIRECTION ( 'NONE',  ( 0.9396926207859063185, 0.3420201433256743750, 0.000000000000000000 ) ) ;
#1097 = EDGE_CURVE ( 'NONE', #998, #218, #875, .T. ) ;
#1098 = ORIENTED_EDGE ( 'NONE', *, *, #355, .F. ) ;
#1099 = LINE ( 'NONE', #877, #948 ) ;
#1100 = DIRECTION ( 'NONE',  ( -0.000000000000000000, -0.000000000000000000, 1.000000000000000000 ) ) ;
#1101 = VERTEX_POINT ( 'NONE', #464 ) ;
#1102 = EDGE_CURVE ( 'NONE', #2075, #766, #907, .T. ) ;
#1103 = CARTESIAN_POINT ( 'NONE',  ( -31.00000000000002132, -30.19615242270664268, 6.000000000000000000 ) ) ;
#1104 = DIRECTION ( 'NONE',  ( -0.4999999999999981681, 0.8660254037844397068, -0.000000000000000000 ) ) ;
#1105 = ORIENTED_EDGE ( 'NONE', *, *, #282, .T. ) ;
#1106 = CARTESIAN_POINT ( 'NONE',  ( -49.99038105676663690, -27.30384757729335377, 6.000000000000000000 ) ) ;
#1107 = PRODUCT_DEFINITION ( 'UNKNOWN', '', #1218, #2292 ) ;
#1108 = PLANE ( 'NONE',  #1552 ) ;
#1109 = DIRECTION ( 'NONE',  ( -0.000000000000000000, -1.000000000000000000, -0.000000000000000000 ) ) ;
#1110 = ADVANCED_BREP_SHAPE_REPRESENTATION ( '', ( #2534, #2652 ), #465 ) ;
#1111 = ORIENTED_EDGE ( 'NONE', *, *, #872, .T. ) ;
#1112 = CARTESIAN_POINT ( 'NONE',  ( -54.98076211353320275, 10.00000000000005684, 3.000000000000000000 ) ) ;
#1113 = DIRECTION ( 'NONE',  ( -0.000000000000000000, 1.000000000000000000, -0.000000000000000000 ) ) ;
#1114 = ORIENTED_EDGE ( 'NONE', *, *, #1749, .F. ) ;
#1115 = CONICAL_SURFACE ( 'NONE', #1495, 4.133974596215571395, 0.5235987755983229075 ) ;
#1116 = DIRECTION ( 'NONE',  ( -0.000000000000000000, 1.000000000000000000, -0.000000000000000000 ) ) ;
#1117 = ORIENTED_EDGE ( 'NONE', *, *, #2470, .T. ) ;
#1118 = VECTOR ( 'NONE', #781, 1000.000000000000114 ) ;
#1119 = DIRECTION ( 'NONE',  ( 0.8660254037844398178, 0.4999999999999977796, 0.000000000000000000 ) ) ;
#1120 = DIRECTION ( 'NONE',  ( -0.000000000000000000, -0.000000000000000000, 1.000000000000000000 ) ) ;
#1121 = EDGE_CURVE ( 'NONE', #2433, #81, #1088, .T. ) ;
#1122 = CARTESIAN_POINT ( 'NONE',  ( -31.00000000000008171, -50.19615242270659650, 3.000000000000002220 ) ) ;
#1123 = VECTOR ( 'NONE', #676, 1000.000000000000000 ) ;
#1124 = CIRCLE ( 'NONE', #2810, 5.000000000000000000 ) ;
#1125 = ORIENTED_EDGE ( 'NONE', *, *, #2417, .F. ) ;
#1126 = CARTESIAN_POINT ( 'NONE',  ( 0.000000000000000000, -149.1719999999999970, 5.000000000000000000 ) ) ;
#1127 = DIRECTION ( 'NONE',  ( 1.000000000000000000, 0.000000000000000000, 0.000000000000000000 ) ) ;
#1128 = EDGE_LOOP ( 'NONE', ( #1388, #2021, #1429, #2033 ) ) ;
#1129 = LINE ( 'NONE', #2046, #2025 ) ;
#1130 = AXIS2_PLACEMENT_3D ( 'NONE', #1868, #604, #2862 ) ;
#1131 = CARTESIAN_POINT ( 'NONE',  ( -39.66025403784451697, -55.19615242270660360, -2.999999999999998224 ) ) ;
#1132 = EDGE_CURVE ( 'NONE', #705, #1494, #71, .T. ) ;
#1133 = ORIENTED_EDGE ( 'NONE', *, *, #2872, .T. ) ;
#1134 = CARTESIAN_POINT ( 'NONE',  ( -59.98076211353318854, -69.99999999999995737, -3.000000000000005329 ) ) ;
#1135 = AXIS2_PLACEMENT_3D ( 'NONE', #2635, #352, #2407 ) ;
#1136 = DIRECTION ( 'NONE',  ( 1.000000000000000000, 0.000000000000000000, -1.502314598737159524E-16 ) ) ;
#1137 = PLANE ( 'NONE',  #11 ) ;
#1138 = EDGE_CURVE ( 'NONE', #776, #915, #5, .T. ) ;
#1139 = VERTEX_POINT ( 'NONE', #1368 ) ;
#1140 = FACE_OUTER_BOUND ( 'NONE', #2387, .T. ) ;
#1141 = ITEM_DEFINED_TRANSFORMATION ( 'NONE', 'NONE', #2461,  #2652 ) ;
#1142 = DIRECTION ( 'NONE',  ( 1.000000000000000000, 0.000000000000000000, 0.000000000000000000 ) ) ;
#1143 = ORIENTED_EDGE ( 'NONE', *, *, #1904, .F. ) ;
#1144 = CARTESIAN_POINT ( 'NONE',  ( -36.64999999999999147, -25.00000000000000000, 6.000000000000000000 ) ) ;
#1145 = FILL_AREA_STYLE_COLOUR ( '', #2125 ) ;
#1146 = ORIENTED_EDGE ( 'NONE', *, *, #282, .F. ) ;
#1147 = CARTESIAN_POINT ( 'NONE',  ( -34.99999999999999289, -24.99999999999999645, 3.000000000000000000 ) ) ;
#1148 = SURFACE_STYLE_FILL_AREA ( #104 ) ;
#1149 = DIRECTION ( 'NONE',  ( -1.000000000000000000, 0.000000000000000000, 0.000000000000000000 ) ) ;
#1150 = DIRECTION ( 'NONE',  ( -0.000000000000000000, -1.000000000000000000, -0.000000000000000000 ) ) ;
#1151 = ORIENTED_EDGE ( 'NONE', *, *, #462, .F. ) ;
#1152 = DIRECTION ( 'NONE',  ( 0.000000000000000000, 0.000000000000000000, 1.000000000000000000 ) ) ;
#1153 = DIRECTION ( 'NONE',  ( 0.000000000000000000, 1.000000000000000000, 0.000000000000000000 ) ) ;
#1154 = EDGE_LOOP ( 'NONE', ( #2301, #995, #1242, #2705 ) ) ;
#1155 = EDGE_CURVE ( 'NONE', #730, #1818, #2672, .T. ) ;
#1156 = CARTESIAN_POINT ( 'NONE',  ( 0.000000000000000000, -1.999999999999980016, 4.999999999999998224 ) ) ;
#1157 = DIRECTION ( 'NONE',  ( -0.000000000000000000, -1.000000000000000000, -0.000000000000000000 ) ) ;
#1158 = ORIENTED_EDGE ( 'NONE', *, *, #65, .T. ) ;
#1159 = DIRECTION ( 'NONE',  ( 1.000000000000000000, 0.000000000000000000, 0.000000000000000000 ) ) ;
#1160 = VECTOR ( 'NONE', #745, 1000.000000000000000 ) ;
#1161 = DIRECTION ( 'NONE',  ( 0.4999999999999981681, -0.8660254037844397068, 0.000000000000000000 ) ) ;
#1162 = VECTOR ( 'NONE', #1050, 1000.000000000000000 ) ;
#1163 = FACE_OUTER_BOUND ( 'NONE', #47, .T. ) ;
#1164 = EDGE_CURVE ( 'NONE', #93, #2315, #2008, .T. ) ;
#1165 = CARTESIAN_POINT ( 'NONE',  ( -36.99999999999999289, -19.80384757729336087, 6.000000000000000000 ) ) ;
#1166 = ORIENTED_EDGE ( 'NONE', *, *, #2153, .T. ) ;
#1167 = CARTESIAN_POINT ( 'NONE',  ( -37.91455138073065001, -142.8479302707733041, 3.000000000000000000 ) ) ;
#1168 = VECTOR ( 'NONE', #2020, 1000.000000000000000 ) ;
#1169 = DIRECTION ( 'NONE',  ( 0.4999999999999977796, -0.8660254037844398178, 0.000000000000000000 ) ) ;
#1170 =( GEOMETRIC_REPRESENTATION_CONTEXT ( 3 ) GLOBAL_UNCERTAINTY_ASSIGNED_CONTEXT ( ( #1831 ) ) GLOBAL_UNIT_ASSIGNED_CONTEXT ( ( #1477, #2599, #2403 ) ) REPRESENTATION_CONTEXT ( 'NONE', 'WORKASPACE' ) );
#1171 = ORIENTED_EDGE ( 'NONE', *, *, #1530, .F. ) ;
#1172 = FACE_OUTER_BOUND ( 'NONE', #980, .T. ) ;
#1173 = TOROIDAL_SURFACE ( 'NONE', #2177, 4.999999999999998224, 0.9999999999999995559 ) ;
#1174 = EDGE_CURVE ( 'NONE', #1517, #862, #2892, .T. ) ;
#1175 = CARTESIAN_POINT ( 'NONE',  ( 40.00000000000000711, -24.99999999999999645, -3.000000000000000888 ) ) ;
#1176 = ADVANCED_BREP_SHAPE_REPRESENTATION ( '', ( #1577, #2652 ), #2217 ) ;
#1177 = ORIENTED_EDGE ( 'NONE', *, *, #2449, .F. ) ;
#1178 = DIRECTION ( 'NONE',  ( -0.8660254037844398178, -0.4999999999999977796, 1.469576158976821827E-16 ) ) ;
#1179 = AXIS2_PLACEMENT_3D ( 'NONE', #1498, #847, #2190 ) ;
#1180 = DIRECTION ( 'NONE',  ( 1.076523719386531503E-16, 6.215312591768280423E-17, -1.000000000000000000 ) ) ;
#1181 = CARTESIAN_POINT ( 'NONE',  ( -39.99999999999999289, -30.00000000000000000, 3.000000000000000000 ) ) ;
#1182 = DIRECTION ( 'NONE',  ( 0.000000000000000000, 1.000000000000000000, 0.000000000000000000 ) ) ;
#1183 = VECTOR ( 'NONE', #2772, 1000.000000000000000 ) ;
#1184 = PRODUCT_DEFINITION_SHAPE ( 'NONE', 'NONE',  #1107 ) ;
#1185 = ORIENTED_EDGE ( 'NONE', *, *, #2682, .F. ) ;
#1186 = EDGE_CURVE ( 'NONE', #2206, #1884, #2440, .T. ) ;
#1187 = DIRECTION ( 'NONE',  ( -1.000000000000000000, 0.000000000000000000, 8.673617379884040402E-17 ) ) ;
#1188 = EDGE_CURVE ( 'NONE', #1027, #2297, #1989, .T. ) ;
#1189 = CARTESIAN_POINT ( 'NONE',  ( -62.63076211353318712, -9.999999999999943157, -3.000000000000005329 ) ) ;
#1190 = EDGE_LOOP ( 'NONE', ( #1875, #1724, #1194, #277 ) ) ;
#1191 = CARTESIAN_POINT ( 'NONE',  ( -46.49038105676660848, -33.36602540378440551, 3.000000000000002220 ) ) ;
#1192 = DIRECTION ( 'NONE',  ( 0.000000000000000000, 0.000000000000000000, 1.000000000000000000 ) ) ;
#1193 = EDGE_CURVE ( 'NONE', #1630, #1931, #2463, .T. ) ;
#1194 = ORIENTED_EDGE ( 'NONE', *, *, #1702, .T. ) ;
#1195 = ADVANCED_FACE ( 'NONE', ( #2929 ), #635, .T. ) ;
#1196 = CARTESIAN_POINT ( 'NONE',  ( 35.00000000000002132, -25.00000000000000000, 3.000000000000000000 ) ) ;
#1197 = DIRECTION ( 'NONE',  ( 1.000000000000000000, 0.000000000000000000, 1.224646799147353207E-16 ) ) ;
#1198 = DIRECTION ( 'NONE',  ( -0.4999999999999981681, 0.8660254037844397068, 0.000000000000000000 ) ) ;
#1199 = LINE ( 'NONE', #268, #1313 ) ;
#1200 = PRODUCT_RELATED_PRODUCT_CATEGORY ( 'part', '', ( #1586 ) ) ;
#1201 = EDGE_CURVE ( 'NONE', #2405, #1292, #2578, .T. ) ;
#1202 = ORIENTED_EDGE ( 'NONE', *, *, #532, .F. ) ;
#1203 = FACE_OUTER_BOUND ( 'NONE', #1737, .T. ) ;
#1204 = VERTEX_POINT ( 'NONE', #2295 ) ;
#1205 = DIRECTION ( 'NONE',  ( -0.4999999999999972244, 0.8660254037844402619, 0.000000000000000000 ) ) ;
#1206 = DIRECTION ( 'NONE',  ( 0.8660254037844404840, 0.4999999999999968914, -0.000000000000000000 ) ) ;
#1207 = ORIENTED_EDGE ( 'NONE', *, *, #1276, .F. ) ;
#1208 = DIRECTION ( 'NONE',  ( 0.000000000000000000, 0.000000000000000000, 1.000000000000000000 ) ) ;
#1209 = UNCERTAINTY_MEASURE_WITH_UNIT (LENGTH_MEASURE( 1.000000000000000082E-05 ), #1985, 'distance_accuracy_value', 'NONE');
#1210 = PLANE ( 'NONE',  #1213 ) ;
#1211 = ORIENTED_EDGE ( 'NONE', *, *, #1935, .T. ) ;
#1212 = AXIS2_PLACEMENT_3D ( 'NONE', #2643, #1709, #2630 ) ;
#1213 = AXIS2_PLACEMENT_3D ( 'NONE', #2532, #279, #1198 ) ;
#1214 = ADVANCED_FACE ( 'NONE', ( #1881 ), #692, .F. ) ;
#1215 = ORIENTED_EDGE ( 'NONE', *, *, #947, .T. ) ;
#1216 = AXIS2_PLACEMENT_3D ( 'NONE', #963, #90, #976 ) ;
#1217 = DIRECTION ( 'NONE',  ( 1.000000000000000000, 0.000000000000000000, 1.636531581110204284E-16 ) ) ;
#1218 = PRODUCT_DEFINITION_FORMATION_WITH_SPECIFIED_SOURCE ( 'ANY', '', #2791, .NOT_KNOWN. ) ;
#1219 = EDGE_LOOP ( 'NONE', ( #1459, #203, #871, #411, #1211, #1046, #2542, #1438, #320 ) ) ;
#1220 = AXIS2_PLACEMENT_3D ( 'NONE', #313, #753, #951 ) ;
#1221 = DIRECTION ( 'NONE',  ( -0.000000000000000000, -0.000000000000000000, 1.000000000000000000 ) ) ;
#1222 = MECHANICAL_DESIGN_GEOMETRIC_PRESENTATION_REPRESENTATION (  '', ( #2563 ), #1170 ) ;
#1223 = DIRECTION ( 'NONE',  ( 1.000000000000000000, 0.000000000000000000, 0.000000000000000000 ) ) ;
#1224 = ORIENTED_EDGE ( 'NONE', *, *, #2639, .F. ) ;
#1225 =( NAMED_UNIT ( * ) SI_UNIT ( $, .STERADIAN. ) SOLID_ANGLE_UNIT ( ) );
#1226 = AXIS2_PLACEMENT_3D ( 'NONE', #1911, #543, #2398 ) ;
#1227 = CARTESIAN_POINT ( 'NONE',  ( -31.35000000000000853, -25.00000000000000000, 3.000000000000000000 ) ) ;
#1228 = EDGE_CURVE ( 'NONE', #2206, #2636, #2111, .T. ) ;
#1229 = EDGE_LOOP ( 'NONE', ( #720, #2771, #2825, #2871 ) ) ;
#1230 = AXIS2_PLACEMENT_3D ( 'NONE', #2104, #770, #742 ) ;
#1231 =( NAMED_UNIT ( * ) SI_UNIT ( $, .STERADIAN. ) SOLID_ANGLE_UNIT ( ) );
#1232 = CIRCLE ( 'NONE', #952, 4.999999999999997335 ) ;
#1233 = ORIENTED_EDGE ( 'NONE', *, *, #28, .T. ) ;
#1234 = ADVANCED_FACE ( 'NONE', ( #2307 ), #2083, .F. ) ;
#1235 = VECTOR ( 'NONE', #1109, 1000.000000000000000 ) ;
#1236 = CARTESIAN_POINT ( 'NONE',  ( -62.63076211353317291, -39.99999999999994316, 6.000000000000000000 ) ) ;
#1237 = LINE ( 'NONE', #2146, #2666 ) ;
#1238 = DIRECTION ( 'NONE',  ( -0.000000000000000000, 1.000000000000000000, -0.000000000000000000 ) ) ;
#1239 = ORIENTED_EDGE ( 'NONE', *, *, #1095, .F. ) ;
#1240 = FACE_BOUND ( 'NONE', #2054, .T. ) ;
#1241 = CARTESIAN_POINT ( 'NONE',  ( -59.98076211353319565, -9.999999999999943157, 3.000000000000001332 ) ) ;
#1242 = ORIENTED_EDGE ( 'NONE', *, *, #1342, .F. ) ;
#1243 = CARTESIAN_POINT ( 'NONE',  ( 0.000000000000000000, -30.00000000000000000, 0.000000000000000000 ) ) ;
#1244 = ORIENTED_EDGE ( 'NONE', *, *, #1840, .T. ) ;
#1245 = CARTESIAN_POINT ( 'NONE',  ( 0.000000000000000000, -20.00000000000000000, 0.000000000000000000 ) ) ;
#1246 = DIRECTION ( 'NONE',  ( -0.000000000000000000, -1.000000000000000000, -0.000000000000000000 ) ) ;
#1247 = LINE ( 'NONE', #555, #2262 ) ;
#1248 = ADVANCED_FACE ( 'NONE', ( #2533, #2743 ), #711, .F. ) ;
#1249 = VERTEX_POINT ( 'NONE', #1834 ) ;
#1250 = PLANE ( 'NONE',  #1268 ) ;
#1251 = CARTESIAN_POINT ( 'NONE',  ( 0.000000000000000000, -149.1719999999999970, 0.000000000000000000 ) ) ;
#1252 = VERTEX_POINT ( 'NONE', #538 ) ;
#1253 = CARTESIAN_POINT ( 'NONE',  ( -59.98076211353318854, -39.99999999999994316, -3.000000000000005329 ) ) ;
#1254 =( LENGTH_UNIT ( ) NAMED_UNIT ( * ) SI_UNIT ( .MILLI., .METRE. ) );
#1255 = ADVANCED_FACE ( 'NONE', ( #45 ), #1463, .T. ) ;
#1256 = ORIENTED_EDGE ( 'NONE', *, *, #1085, .F. ) ;
#1257 = CARTESIAN_POINT ( 'NONE',  ( -6.873863542433761076, -20.00000000000000000, -3.000000000000000000 ) ) ;
#1258 = ORIENTED_EDGE ( 'NONE', *, *, #2481, .F. ) ;
#1259 = CARTESIAN_POINT ( 'NONE',  ( -26.66987298107781257, -27.69615242270665689, -3.000000000000000000 ) ) ;
#1260 = STYLED_ITEM ( 'NONE', ( #1770 ), #1176 ) ;
#1261 = CARTESIAN_POINT ( 'NONE',  ( 5.773502691896260863, 13.00000000000000178, 9.999999999999998224 ) ) ;
#1262 = ORIENTED_EDGE ( 'NONE', *, *, #607, .T. ) ;
#1263 = AXIS2_PLACEMENT_3D ( 'NONE', #281, #1399, #1662 ) ;
#1264 = EDGE_CURVE ( 'NONE', #2799, #1101, #838, .T. ) ;
#1265 = DIRECTION ( 'NONE',  ( 0.000000000000000000, 0.000000000000000000, 1.000000000000000000 ) ) ;
#1266 = EDGE_CURVE ( 'NONE', #1931, #1058, #1414, .T. ) ;
#1267 = DIRECTION ( 'NONE',  ( 2.312964634635742661E-15, -0.000000000000000000, 1.000000000000000000 ) ) ;
#1268 = AXIS2_PLACEMENT_3D ( 'NONE', #2195, #2149, #2165 ) ;
#1269 = ORIENTED_EDGE ( 'NONE', *, *, #2785, .T. ) ;
#1270 = FACE_OUTER_BOUND ( 'NONE', #2023, .T. ) ;
#1271 = CIRCLE ( 'NONE', #1370, 15.00000000000000178 ) ;
#1272 = FILL_AREA_STYLE_COLOUR ( '', #466 ) ;
#1273 = ORIENTED_EDGE ( 'NONE', *, *, #624, .T. ) ;
#1274 = VECTOR ( 'NONE', #1301, 1000.000000000000000 ) ;
#1275 = SURFACE_SIDE_STYLE ('',( #845 ) ) ;
#1276 = EDGE_CURVE ( 'NONE', #1425, #737, #494, .T. ) ;
#1277 = CARTESIAN_POINT ( 'NONE',  ( -34.99999999999999289, -25.00000000000000000, 0.000000000000000000 ) ) ;
#1278 = FACE_OUTER_BOUND ( 'NONE', #432, .T. ) ;
#1279 = EDGE_LOOP ( 'NONE', ( #530, #2658 ) ) ;
#1280 = CARTESIAN_POINT ( 'NONE',  ( 0.000000000000000000, -1.999999999999980016, 0.000000000000000000 ) ) ;
#1281 = DIRECTION ( 'NONE',  ( 0.5000000000000004441, 0.000000000000000000, 0.8660254037844383745 ) ) ;
#1282 = ORIENTED_EDGE ( 'NONE', *, *, #1632, .T. ) ;
#1283 = DIRECTION ( 'NONE',  ( 0.000000000000000000, 0.000000000000000000, 1.000000000000000000 ) ) ;
#1284 = EDGE_CURVE ( 'NONE', #969, #814, #2127, .T. ) ;
#1285 = SURFACE_STYLE_FILL_AREA ( #2423 ) ;
#1286 = EDGE_CURVE ( 'NONE', #2075, #2839, #1199, .T. ) ;
#1287 = ORIENTED_EDGE ( 'NONE', *, *, #2757, .T. ) ;
#1288 = EDGE_LOOP ( 'NONE', ( #759, #2631, #1233, #2088 ) ) ;
#1289 = CYLINDRICAL_SURFACE ( 'NONE', #343, 7.500000000000000888 ) ;
#1290 = DIRECTION ( 'NONE',  ( 0.000000000000000000, 0.000000000000000000, 1.000000000000000000 ) ) ;
#1291 = LINE ( 'NONE', #2238, #2119 ) ;
#1292 = VERTEX_POINT ( 'NONE', #2341 ) ;
#1293 = LINE ( 'NONE', #834, #2324 ) ;
#1294 = ORIENTED_EDGE ( 'NONE', *, *, #1007, .F. ) ;
#1295 = DIRECTION ( 'NONE',  ( 1.000000000000000000, 0.000000000000000000, 0.000000000000000000 ) ) ;
#1296 = CARTESIAN_POINT ( 'NONE',  ( 0.000000000000000000, 3.000000000000000000, -15.00000000000000178 ) ) ;
#1297 = CARTESIAN_POINT ( 'NONE',  ( 5.773502691896260863, 13.00000000000000178, 9.999999999999998224 ) ) ;
#1298 = EDGE_LOOP ( 'NONE', ( #2796, #1177 ) ) ;
#1299 = ADVANCED_FACE ( 'NONE', ( #2099 ), #935, .F. ) ;
#1300 = FILL_AREA_STYLE_COLOUR ( '', #1824 ) ;
#1301 = DIRECTION ( 'NONE',  ( 0.9396926207859063185, 0.3420201433256743750, 0.000000000000000000 ) ) ;
#1302 = VECTOR ( 'NONE', #2012, 1000.000000000000000 ) ;
#1303 = DIRECTION ( 'NONE',  ( 0.000000000000000000, 0.000000000000000000, 1.000000000000000000 ) ) ;
#1304 = FACE_OUTER_BOUND ( 'NONE', #1611, .T. ) ;
#1305 = VECTOR ( 'NONE', #580, 1000.000000000000000 ) ;
#1306 = EDGE_LOOP ( 'NONE', ( #2804, #1970 ) ) ;
#1307 = AXIS2_PLACEMENT_3D ( 'NONE', #350, #1726, #835 ) ;
#1308 = CARTESIAN_POINT ( 'NONE',  ( -32.66987298107778059, -17.30384757729337508, 6.000000000000000000 ) ) ;
#1309 = DIRECTION ( 'NONE',  ( 1.000000000000000000, 0.000000000000000000, 0.000000000000000000 ) ) ;
#1310 = AXIS2_PLACEMENT_3D ( 'NONE', #2690, #1025, #1499 ) ;
#1311 = EDGE_CURVE ( 'NONE', #391, #1425, #1853, .T. ) ;
#1312 = ORIENTED_EDGE ( 'NONE', *, *, #1763, .T. ) ;
#1313 = VECTOR ( 'NONE', #524, 1000.000000000000000 ) ;
#1314 = CARTESIAN_POINT ( 'NONE',  ( -5.773502691896258199, 3.000000000000000000, -9.999999999999998224 ) ) ;
#1315 = ADVANCED_FACE ( 'NONE', ( #79, #965, #1163 ), #2790, .T. ) ;
#1316 = DIRECTION ( 'NONE',  ( 1.224646799147352468E-16, 0.000000000000000000, -1.000000000000000000 ) ) ;
#1317 = AXIS2_PLACEMENT_3D ( 'NONE', #2002, #1331, #205 ) ;
#1318 = DIRECTION ( 'NONE',  ( -1.000000000000000000, -0.000000000000000000, -0.000000000000000000 ) ) ;
#1319 = DIRECTION ( 'NONE',  ( 1.000000000000000000, 0.000000000000000000, 0.000000000000000000 ) ) ;
#1320 = AXIS2_PLACEMENT_3D ( 'NONE', #1464, #2816, #970 ) ;
#1321 = ADVANCED_FACE ( 'NONE', ( #2354 ), #1137, .F. ) ;
#1322 = ORIENTED_EDGE ( 'NONE', *, *, #895, .T. ) ;
#1323 = CARTESIAN_POINT ( 'NONE',  ( -34.99999999999999289, -20.00000000000000000, -3.000000000000000000 ) ) ;
#1324 = VECTOR ( 'NONE', #284, 1000.000000000000000 ) ;
#1325 = CONTEXT_DEPENDENT_SHAPE_REPRESENTATION ( #841, #2447 ) ;
#1326 = DIRECTION ( 'NONE',  ( 8.659560562354961208E-17, 0.7071067811865452413, -0.7071067811865497932 ) ) ;
#1327 = AXIS2_PLACEMENT_3D ( 'NONE', #362, #393, #2876 ) ;
#1328 = EDGE_CURVE ( 'NONE', #349, #2171, #1988, .T. ) ;
#1329 = ORIENTED_EDGE ( 'NONE', *, *, #2351, .F. ) ;
#1330 = AXIS2_PLACEMENT_3D ( 'NONE', #2474, #238, #194 ) ;
#1331 = DIRECTION ( 'NONE',  ( -1.272690286469888396E-16, -7.347880794884083251E-17, -1.000000000000000000 ) ) ;
#1332 = VERTEX_POINT ( 'NONE', #906 ) ;
#1333 = DIRECTION ( 'NONE',  ( 1.000000000000000000, 0.000000000000000000, 8.673617379884040402E-17 ) ) ;
#1334 = UNCERTAINTY_MEASURE_WITH_UNIT (LENGTH_MEASURE( 1.000000000000000082E-05 ), #778, 'distance_accuracy_value', 'NONE');
#1335 = DIRECTION ( 'NONE',  ( -1.000000000000000000, 0.000000000000000000, 0.000000000000000000 ) ) ;
#1336 = APPLICATION_CONTEXT ( 'automotive_design' ) ;
#1337 = DIRECTION ( 'NONE',  ( -0.8660254037844401509, -0.4999999999999971689, 1.469576158976821827E-16 ) ) ;
#1338 = EDGE_LOOP ( 'NONE', ( #1282, #438 ) ) ;
#1339 = PLANE ( 'NONE',  #564 ) ;
#1340 = LINE ( 'NONE', #1734, #236 ) ;
#1341 = EDGE_LOOP ( 'NONE', ( #2912, #1696, #1648, #1407 ) ) ;
#1342 = EDGE_CURVE ( 'NONE', #608, #167, #1649, .T. ) ;
#1343 = DIRECTION ( 'NONE',  ( -0.8660254037844398178, -0.4999999999999977796, 0.000000000000000000 ) ) ;
#1344 = SURFACE_STYLE_FILL_AREA ( #2185 ) ;
#1345 = ORIENTED_EDGE ( 'NONE', *, *, #597, .T. ) ;
#1346 = DIRECTION ( 'NONE',  ( 0.000000000000000000, 1.000000000000000000, 0.000000000000000000 ) ) ;
#1347 = FACE_BOUND ( 'NONE', #1620, .T. ) ;
#1348 = EDGE_CURVE ( 'NONE', #1049, #2555, #2607, .T. ) ;
#1349 = ORIENTED_EDGE ( 'NONE', *, *, #925, .F. ) ;
#1350 = CARTESIAN_POINT ( 'NONE',  ( 0.000000000000000000, -150.0000000000000000, 4.171999999999999709 ) ) ;
#1351 = ORIENTED_EDGE ( 'NONE', *, *, #233, .T. ) ;
#1352 = FACE_OUTER_BOUND ( 'NONE', #290, .T. ) ;
#1353 = SHAPE_DEFINITION_REPRESENTATION ( #1870, #1689 ) ;
#1354 = ADVANCED_FACE ( 'NONE', ( #2487 ), #1108, .F. ) ;
#1355 = FACE_BOUND ( 'NONE', #1525, .T. ) ;
#1356 = AXIS2_PLACEMENT_3D ( 'NONE', #1821, #453, #286 ) ;
#1357 = ORIENTED_EDGE ( 'NONE', *, *, #1012, .T. ) ;
#1358 = VECTOR ( 'NONE', #2234, 1000.000000000000114 ) ;
#1359 = CARTESIAN_POINT ( 'NONE',  ( 0.000000000000000000, -150.0000000000000000, 0.000000000000000000 ) ) ;
#1360 = DIRECTION ( 'NONE',  ( -1.272690286469888396E-16, -7.347880794884083251E-17, -1.000000000000000000 ) ) ;
#1361 = ORIENTED_EDGE ( 'NONE', *, *, #1897, .T. ) ;
#1362 = CIRCLE ( 'NONE', #1460, 3.999999999999998224 ) ;
#1363 = ADVANCED_FACE ( 'NONE', ( #647 ), #1583, .F. ) ;
#1364 = DIRECTION ( 'NONE',  ( 1.000000000000000000, 0.000000000000000000, 0.000000000000000000 ) ) ;
#1365 = UNCERTAINTY_MEASURE_WITH_UNIT (LENGTH_MEASURE( 1.000000000000000082E-05 ), #1254, 'distance_accuracy_value', 'NONE');
#1366 = CARTESIAN_POINT ( 'NONE',  ( 5.773502691896257311, 3.000000000000000000, -10.00000000000000000 ) ) ;
#1367 = AXIS2_PLACEMENT_3D ( 'NONE', #587, #2842, #1490 ) ;
#1368 = CARTESIAN_POINT ( 'NONE',  ( -61.31088913245546479, -47.69615242270656807, 3.000000000000000000 ) ) ;
#1369 = VECTOR ( 'NONE', #2541, 1000.000000000000000 ) ;
#1370 = AXIS2_PLACEMENT_3D ( 'NONE', #306, #1845, #1192 ) ;
#1371 = VERTEX_POINT ( 'NONE', #447 ) ;
#1372 = DIRECTION ( 'NONE',  ( -0.000000000000000000, 1.000000000000000000, -0.000000000000000000 ) ) ;
#1373 = VECTOR ( 'NONE', #356, 1000.000000000000000 ) ;
#1374 = FACE_BOUND ( 'NONE', #2738, .T. ) ;
#1375 = EDGE_CURVE ( 'NONE', #2179, #2824, #2270, .T. ) ;
#1376 = CARTESIAN_POINT ( 'NONE',  ( -41.49038105676660848, -33.36602540378440551, 3.000000000000002220 ) ) ;
#1377 = AXIS2_PLACEMENT_3D ( 'NONE', #1485, #1205, #2836 ) ;
#1378 = DIRECTION ( 'NONE',  ( -0.000000000000000000, -0.000000000000000000, -1.000000000000000000 ) ) ;
#1379 = VECTOR ( 'NONE', #2894, 1000.000000000000000 ) ;
#1380 = ORIENTED_EDGE ( 'NONE', *, *, #1264, .T. ) ;
#1381 = LINE ( 'NONE', #42, #210 ) ;
#1382 = CIRCLE ( 'NONE', #2285, 2.649999999999992806 ) ;
#1383 = CARTESIAN_POINT ( 'NONE',  ( -47.49038105676664401, -31.63397459621555186, -2.999999999999999112 ) ) ;
#1384 = VERTEX_POINT ( 'NONE', #1539 ) ;
#1385 = DIRECTION ( 'NONE',  ( -1.000000000000000000, 0.000000000000000000, 0.000000000000000000 ) ) ;
#1386 = ADVANCED_FACE ( 'NONE', ( #1554, #31 ), #917, .F. ) ;
#1387 = PRODUCT_DEFINITION ( 'UNKNOWN', '', #1028, #887 ) ;
#1388 = ORIENTED_EDGE ( 'NONE', *, *, #1866, .F. ) ;
#1389 = FACE_OUTER_BOUND ( 'NONE', #1964, .T. ) ;
#1390 = PLANE ( 'NONE',  #1877 ) ;
#1391 = ORIENTED_EDGE ( 'NONE', *, *, #799, .T. ) ;
#1392 = DIRECTION ( 'NONE',  ( 0.000000000000000000, 0.000000000000000000, 1.000000000000000000 ) ) ;
#1393 = LINE ( 'NONE', #2091, #2356 ) ;
#1394 = ORIENTED_EDGE ( 'NONE', *, *, #1749, .T. ) ;
#1395 = CARTESIAN_POINT ( 'NONE',  ( -54.98076211353318143, -128.6602540378443393, 3.000000000000000000 ) ) ;
#1396 = SHAPE_REPRESENTATION ( 'Jaw Forging Puller Arm', ( #2652 ), #986 ) ;
#1397 = CARTESIAN_POINT ( 'NONE',  ( -54.98076211353320275, 10.00000000000005684, -3.000000000000000000 ) ) ;
#1398 = LINE ( 'NONE', #1864, #2504 ) ;
#1399 = DIRECTION ( 'NONE',  ( -0.000000000000000000, -0.000000000000000000, 1.000000000000000000 ) ) ;
#1400 = EDGE_LOOP ( 'NONE', ( #1777, #1476, #1991, #2897, #2582, #668, #1757, #884, #2384 ) ) ;
#1401 = DIRECTION ( 'NONE',  ( 0.000000000000000000, 0.000000000000000000, 1.000000000000000000 ) ) ;
#1402 = ADVANCED_FACE ( 'NONE', ( #1347, #1804, #874 ), #1759, .F. ) ;
#1403 = DIRECTION ( 'NONE',  ( 0.000000000000000000, 0.000000000000000000, -1.000000000000000000 ) ) ;
#1404 = ORIENTED_EDGE ( 'NONE', *, *, #1000, .T. ) ;
#1405 = ORIENTED_EDGE ( 'NONE', *, *, #233, .F. ) ;
#1406 = LINE ( 'NONE', #2510, #2568 ) ;
#1407 = ORIENTED_EDGE ( 'NONE', *, *, #2915, .F. ) ;
#1408 = DIRECTION ( 'NONE',  ( 1.000000000000000000, 0.000000000000000000, 1.636531581110204284E-16 ) ) ;
#1409 = CIRCLE ( 'NONE', #2885, 15.00000000000000178 ) ;
#1410 = LINE ( 'NONE', #2788, #1504 ) ;
#1411 = FACE_OUTER_BOUND ( 'NONE', #188, .T. ) ;
#1412 = EDGE_CURVE ( 'NONE', #2728, #957, #939, .T. ) ;
#1413 = VECTOR ( 'NONE', #60, 1000.000000000000114 ) ;
#1414 = LINE ( 'NONE', #506, #469 ) ;
#1415 = ADVANCED_FACE ( 'NONE', ( #2730 ), #860, .F. ) ;
#1416 = VECTOR ( 'NONE', #1104, 1000.000000000000000 ) ;
#1417 = EDGE_LOOP ( 'NONE', ( #797, #767, #2780, #1466 ) ) ;
#1418 = ORIENTED_EDGE ( 'NONE', *, *, #1615, .F. ) ;
#1419 = CARTESIAN_POINT ( 'NONE',  ( -26.66987298107781967, -27.69615242270666045, 6.000000000000000000 ) ) ;
#1420 = COLOUR_RGB ( '',0.8941176470588234615, 0.8941176470588234615, 0.8941176470588234615 ) ;
#1421 = DIRECTION ( 'NONE',  ( -0.000000000000000000, -0.000000000000000000, 1.000000000000000000 ) ) ;
#1422 = AXIS2_PLACEMENT_3D ( 'NONE', #2726, #1070, #2483 ) ;
#1423 = EDGE_CURVE ( 'NONE', #876, #2824, #1773, .T. ) ;
#1424 = ORIENTED_EDGE ( 'NONE', *, *, #1493, .T. ) ;
#1425 = VERTEX_POINT ( 'NONE', #1366 ) ;
#1426 = CARTESIAN_POINT ( 'NONE',  ( -5.773502691896258199, 13.00000000000000178, -9.999999999999998224 ) ) ;
#1427 = AXIS2_PLACEMENT_3D ( 'NONE', #944, #489, #2572 ) ;
#1428 = EDGE_CURVE ( 'NONE', #732, #908, #1926, .T. ) ;
#1429 = ORIENTED_EDGE ( 'NONE', *, *, #752, .T. ) ;
#1430 = DIRECTION ( 'NONE',  ( -0.5000000000000013323, 0.8660254037844378194, 0.000000000000000000 ) ) ;
#1431 = CIRCLE ( 'NONE', #63, 8.000000000000000000 ) ;
#1432 =( LENGTH_UNIT ( ) NAMED_UNIT ( * ) SI_UNIT ( .MILLI., .METRE. ) );
#1433 = CARTESIAN_POINT ( 'NONE',  ( -26.66987298107781967, -27.69615242270666045, 6.000000000000000000 ) ) ;
#1434 = DIRECTION ( 'NONE',  ( -0.000000000000000000, -0.000000000000000000, -1.000000000000000000 ) ) ;
#1435 = AXIS2_PLACEMENT_3D ( 'NONE', #1243, #2795, #1059 ) ;
#1436 = EDGE_LOOP ( 'NONE', ( #643, #1357, #2693, #2857 ) ) ;
#1437 = DIRECTION ( 'NONE',  ( 0.000000000000000000, 0.000000000000000000, 1.000000000000000000 ) ) ;
#1438 = ORIENTED_EDGE ( 'NONE', *, *, #2428, .T. ) ;
#1439 = FACE_OUTER_BOUND ( 'NONE', #373, .T. ) ;
#1440 = DIRECTION ( 'NONE',  ( 0.000000000000000000, 1.000000000000000000, 0.000000000000000000 ) ) ;
#1441 = ORIENTED_EDGE ( 'NONE', *, *, #2863, .T. ) ;
#1442 = CARTESIAN_POINT ( 'NONE',  ( -61.31088913245541505, -47.69615242270656807, 6.000000000000000000 ) ) ;
#1443 = ADVANCED_FACE ( 'NONE', ( #1815 ), #2244, .F. ) ;
#1444 = DIRECTION ( 'NONE',  ( 0.000000000000000000, 0.000000000000000000, 1.000000000000000000 ) ) ;
#1445 = CARTESIAN_POINT ( 'NONE',  ( 0.000000000000000000, -30.00000000000000000, 7.500000000000000888 ) ) ;
#1446 = DIRECTION ( 'NONE',  ( 0.000000000000000000, 0.000000000000000000, 1.000000000000000000 ) ) ;
#1447 = VERTEX_POINT ( 'NONE', #2438 ) ;
#1448 = DIRECTION ( 'NONE',  ( 1.000000000000000000, 0.000000000000000000, 0.000000000000000000 ) ) ;
#1449 = ORIENTED_EDGE ( 'NONE', *, *, #1428, .T. ) ;
#1450 = DIRECTION ( 'NONE',  ( 0.000000000000000000, 0.000000000000000000, -1.000000000000000000 ) ) ;
#1451 = EDGE_CURVE ( 'NONE', #1729, #1842, #404, .T. ) ;
#1452 = CARTESIAN_POINT ( 'NONE',  ( 0.000000000000000000, -0.9999999999999997780, 0.000000000000000000 ) ) ;
#1453 = ORIENTED_EDGE ( 'NONE', *, *, #1854, .T. ) ;
#1454 = DIRECTION ( 'NONE',  ( -1.272690286469888396E-16, -7.347880794884083251E-17, -1.000000000000000000 ) ) ;
#1455 = CARTESIAN_POINT ( 'NONE',  ( 0.000000000000000000, -1.999999999999980016, 0.000000000000000000 ) ) ;
#1456 = ADVANCED_FACE ( 'NONE', ( #1076, #504 ), #1660, .T. ) ;
#1457 = ORIENTED_EDGE ( 'NONE', *, *, #28, .F. ) ;
#1458 = CIRCLE ( 'NONE', #2596, 2.649999999999985700 ) ;
#1459 = ORIENTED_EDGE ( 'NONE', *, *, #1521, .T. ) ;
#1460 = AXIS2_PLACEMENT_3D ( 'NONE', #734, #338, #2063 ) ;
#1461 = DIRECTION ( 'NONE',  ( 0.8660254037844402619, 0.4999999999999971689, 0.000000000000000000 ) ) ;
#1462 = VERTEX_POINT ( 'NONE', #2925 ) ;
#1463 = CONICAL_SURFACE ( 'NONE', #2174, 5.000000000000000000, 0.7853981633974514986 ) ;
#1464 = CARTESIAN_POINT ( 'NONE',  ( -46.49038105676664401, -33.36602540378442683, -2.999999999999997335 ) ) ;
#1465 = DIRECTION ( 'NONE',  ( -0.000000000000000000, -0.000000000000000000, -1.000000000000000000 ) ) ;
#1466 = ORIENTED_EDGE ( 'NONE', *, *, #685, .F. ) ;
#1467 = LINE ( 'NONE', #1507, #1647 ) ;
#1468 = EDGE_LOOP ( 'NONE', ( #2539, #123, #1942, #2591 ) ) ;
#1469 = CARTESIAN_POINT ( 'NONE',  ( 35.00000000000001421, -25.00000000000000000, -8.095376221225103140E-14 ) ) ;
#1470 = EDGE_LOOP ( 'NONE', ( #1349, #1287, #2688, #2379 ) ) ;
#1471 = VECTOR ( 'NONE', #1337, 1000.000000000000114 ) ;
#1472 = EDGE_CURVE ( 'NONE', #132, #1742, #962, .T. ) ;
#1473 = FACE_OUTER_BOUND ( 'NONE', #258, .T. ) ;
#1474 = CARTESIAN_POINT ( 'NONE',  ( -54.98076211353320275, 10.00000000000005684, 3.000000000000000000 ) ) ;
#1475 = LINE ( 'NONE', #1670, #1064 ) ;
#1476 = ORIENTED_EDGE ( 'NONE', *, *, #2826, .T. ) ;
#1477 =( LENGTH_UNIT ( ) NAMED_UNIT ( * ) SI_UNIT ( .MILLI., .METRE. ) );
#1478 = LINE ( 'NONE', #2633, #419 ) ;
#1479 = EDGE_LOOP ( 'NONE', ( #325, #2585, #2640, #2235 ) ) ;
#1480 = DIRECTION ( 'NONE',  ( 1.000000000000000000, 0.000000000000000000, 0.000000000000000000 ) ) ;
#1481 = ORIENTED_EDGE ( 'NONE', *, *, #1138, .T. ) ;
#1482 = APPLICATION_CONTEXT ( 'automotive_design' ) ;
#1483 = CARTESIAN_POINT ( 'NONE',  ( -34.99999999999999289, -30.00000000000000000, 3.000000000000000000 ) ) ;
#1484 = EDGE_CURVE ( 'NONE', #2811, #1462, #1410, .T. ) ;
#1485 = CARTESIAN_POINT ( 'NONE',  ( -31.00000000000002132, -30.19615242270664268, 6.000000000000000000 ) ) ;
#1486 = DIRECTION ( 'NONE',  ( 1.000000000000000000, 0.000000000000000000, 0.000000000000000000 ) ) ;
#1487 = DIRECTION ( 'NONE',  ( 1.000000000000000000, 0.000000000000000000, -3.004629197474320528E-16 ) ) ;
#1488 = ORIENTED_EDGE ( 'NONE', *, *, #2182, .F. ) ;
#1489 = CARTESIAN_POINT ( 'NONE',  ( -64.31088913245535821, -132.4999999999999432, -3.000000000000000000 ) ) ;
#1490 = DIRECTION ( 'NONE',  ( 1.000000000000000000, 0.000000000000000000, 0.000000000000000000 ) ) ;
#1491 = ORIENTED_EDGE ( 'NONE', *, *, #1575, .T. ) ;
#1492 = DIRECTION ( 'NONE',  ( -0.000000000000000000, -0.000000000000000000, 1.000000000000000000 ) ) ;
#1493 = EDGE_CURVE ( 'NONE', #814, #2489, #2758, .T. ) ;
#1494 = VERTEX_POINT ( 'NONE', #1644 ) ;
#1495 = AXIS2_PLACEMENT_3D ( 'NONE', #612, #2708, #2900 ) ;
#1496 = LINE ( 'NONE', #1816, #374 ) ;
#1497 = AXIS2_PLACEMENT_3D ( 'NONE', #758, #2581, #1217 ) ;
#1498 = CARTESIAN_POINT ( 'NONE',  ( 0.000000000000000000, 0.000000000000000000, 0.000000000000000000 ) ) ;
#1499 = DIRECTION ( 'NONE',  ( 1.000000000000000000, 0.000000000000000000, 0.000000000000000000 ) ) ;
#1500 = CONICAL_SURFACE ( 'NONE', #1307, 4.133974596215571395, 0.5235987755983229075 ) ;
#1501 = CARTESIAN_POINT ( 'NONE',  ( -32.66987298107778059, -17.30384757729337508, 6.000000000000000000 ) ) ;
#1502 = PRESENTATION_LAYER_ASSIGNMENT (  '', '', ( #148 ) ) ;
#1503 = VERTEX_POINT ( 'NONE', #949 ) ;
#1504 = VECTOR ( 'NONE', #43, 1000.000000000000000 ) ;
#1505 = EDGE_CURVE ( 'NONE', #1494, #53, #2224, .T. ) ;
#1506 = CYLINDRICAL_SURFACE ( 'NONE', #2896, 4.999999999999997335 ) ;
#1507 = CARTESIAN_POINT ( 'NONE',  ( -52.65063509461111835, -62.69615242270656807, -3.000000000000000000 ) ) ;
#1508 = VERTEX_POINT ( 'NONE', #1397 ) ;
#1509 = CARTESIAN_POINT ( 'NONE',  ( -39.99999999999999289, -30.00000000000000000, 3.000000000000000000 ) ) ;
#1510 =( NAMED_UNIT ( * ) SI_UNIT ( $, .STERADIAN. ) SOLID_ANGLE_UNIT ( ) );
#1511 = VERTEX_POINT ( 'NONE', #2517 ) ;
#1512 = DIRECTION ( 'NONE',  ( -1.000000000000000000, 0.000000000000000000, 0.000000000000000000 ) ) ;
#1513 = DIRECTION ( 'NONE',  ( -0.000000000000000000, 1.000000000000000000, -0.000000000000000000 ) ) ;
#1514 = CIRCLE ( 'NONE', #567, 4.999999999999997335 ) ;
#1515 = PRODUCT_CONTEXT ( 'NONE', #577, 'mechanical' ) ;
#1516 = CARTESIAN_POINT ( 'NONE',  ( -43.99038105676666532, -37.69615242270662492, -2.999999999999997335 ) ) ;
#1517 = VERTEX_POINT ( 'NONE', #2807 ) ;
#1518 = CARTESIAN_POINT ( 'NONE',  ( -59.98076211353318854, -39.99999999999994316, 3.000000000000001332 ) ) ;
#1519 = CARTESIAN_POINT ( 'NONE',  ( 5.773502691896260863, 3.000000000000000000, 9.999999999999998224 ) ) ;
#1520 = ORIENTED_EDGE ( 'NONE', *, *, #1886, .T. ) ;
#1521 = EDGE_CURVE ( 'NONE', #415, #1027, #1851, .T. ) ;
#1522 = CARTESIAN_POINT ( 'NONE',  ( -18.00961894323348389, -42.69615242270662492, -3.000000000000000000 ) ) ;
#1523 = DIRECTION ( 'NONE',  ( 1.000000000000000000, 0.000000000000000000, 0.000000000000000000 ) ) ;
#1524 = DIRECTION ( 'NONE',  ( -0.000000000000000000, -0.000000000000000000, 1.000000000000000000 ) ) ;
#1525 = EDGE_LOOP ( 'NONE', ( #2931, #844 ) ) ;
#1526 = CARTESIAN_POINT ( 'NONE',  ( -43.16025403784440329, -29.13397459621553764, 3.000000000000002220 ) ) ;
#1527 = MANIFOLD_SOLID_BREP ( 'M5 Clearance Hole1', #610 ) ;
#1528 = FACE_OUTER_BOUND ( 'NONE', #718, .T. ) ;
#1529 = DIRECTION ( 'NONE',  ( -1.486905836551548586E-16, 1.000000000000000000, 0.000000000000000000 ) ) ;
#1530 = EDGE_CURVE ( 'NONE', #2225, #2634, #1739, .T. ) ;
#1531 = ORIENTED_EDGE ( 'NONE', *, *, #2785, .F. ) ;
#1532 = ADVANCED_FACE ( 'NONE', ( #722 ), #1628, .T. ) ;
#1533 = LINE ( 'NONE', #1308, #2609 ) ;
#1534 = CARTESIAN_POINT ( 'NONE',  ( -58.09974666316955449, -143.2580143298517328, 3.000000000000000000 ) ) ;
#1535 = PRODUCT ( 'Jaw Forging Puller Arm', 'Jaw Forging Puller Arm', '', ( #2221 ) ) ;
#1536 = ORIENTED_EDGE ( 'NONE', *, *, #152, .T. ) ;
#1537 = CARTESIAN_POINT ( 'NONE',  ( -64.98076211353316012, -131.3397459621555754, -3.000000000000000000 ) ) ;
#1538 = MANIFOLD_SOLID_BREP ( 'M5 Clearance Hole1', #109 ) ;
#1539 = CARTESIAN_POINT ( 'NONE',  ( -57.33076211353321128, -9.999999999999943157, 3.000000000000001332 ) ) ;
#1540 = ADVANCED_FACE ( 'NONE', ( #774 ), #2465, .F. ) ;
#1541 = LINE ( 'NONE', #2455, #1235 ) ;
#1542 = EDGE_LOOP ( 'NONE', ( #2451, #1576, #1003, #2496, #868 ) ) ;
#1543 = DIRECTION ( 'NONE',  ( 0.000000000000000000, -0.000000000000000000, 1.000000000000000000 ) ) ;
#1544 = CIRCLE ( 'NONE', #552, 2.649999999999985700 ) ;
#1545 = DIRECTION ( 'NONE',  ( 0.000000000000000000, 0.000000000000000000, 1.000000000000000000 ) ) ;
#1546 = PRESENTATION_LAYER_ASSIGNMENT (  '', '', ( #97 ) ) ;
#1547 = VERTEX_POINT ( 'NONE', #143 ) ;
#1548 = AXIS2_PLACEMENT_3D ( 'NONE', #1455, #2367, #723 ) ;
#1549 = FACE_OUTER_BOUND ( 'NONE', #1687, .T. ) ;
#1550 = CARTESIAN_POINT ( 'NONE',  ( -34.00000000000000000, -25.00000000000000000, -3.000000000000000888 ) ) ;
#1551 = ORIENTED_EDGE ( 'NONE', *, *, #825, .F. ) ;
#1552 = AXIS2_PLACEMENT_3D ( 'NONE', #2684, #2714, #17 ) ;
#1553 = DIRECTION ( 'NONE',  ( -1.272690286469888396E-16, -7.347880794884083251E-17, -1.000000000000000000 ) ) ;
#1554 = FACE_BOUND ( 'NONE', #229, .T. ) ;
#1555 = CIRCLE ( 'NONE', #840, 4.999999999999997335 ) ;
#1556 = VERTEX_POINT ( 'NONE', #1915 ) ;
#1557 = DIRECTION ( 'NONE',  ( 0.000000000000000000, -0.000000000000000000, 1.000000000000000000 ) ) ;
#1558 = VERTEX_POINT ( 'NONE', #2841 ) ;
#1559 = DIRECTION ( 'NONE',  ( 1.000000000000000000, 0.000000000000000000, 0.000000000000000000 ) ) ;
#1560 = EDGE_CURVE ( 'NONE', #81, #1727, #337, .T. ) ;
#1561 = CIRCLE ( 'NONE', #1130, 4.999999999999997335 ) ;
#1562 = PLANE ( 'NONE',  #931 ) ;
#1563 = AXIS2_PLACEMENT_3D ( 'NONE', #1134, #2017, #1 ) ;
#1564 = ORIENTED_EDGE ( 'NONE', *, *, #2153, .F. ) ;
#1565 = ORIENTED_EDGE ( 'NONE', *, *, #68, .F. ) ;
#1566 = DIRECTION ( 'NONE',  ( -0.000000000000000000, -0.000000000000000000, 1.000000000000000000 ) ) ;
#1567 = ORIENTED_EDGE ( 'NONE', *, *, #799, .F. ) ;
#1568 = DIRECTION ( 'NONE',  ( -0.000000000000000000, -0.000000000000000000, -1.000000000000000000 ) ) ;
#1569 = DIRECTION ( 'NONE',  ( -0.000000000000000000, -0.000000000000000000, 1.000000000000000000 ) ) ;
#1570 = ORIENTED_EDGE ( 'NONE', *, *, #1967, .T. ) ;
#1571 = CARTESIAN_POINT ( 'NONE',  ( -39.99999999999999289, -30.00000000000000000, -3.000000000000000000 ) ) ;
#1572 = ORIENTED_EDGE ( 'NONE', *, *, #2757, .F. ) ;
#1573 = LINE ( 'NONE', #1126, #2856 ) ;
#1574 = CYLINDRICAL_SURFACE ( 'NONE', #2122, 8.000000000000000000 ) ;
#1575 = EDGE_CURVE ( 'NONE', #570, #2318, #150, .T. ) ;
#1576 = ORIENTED_EDGE ( 'NONE', *, *, #825, .T. ) ;
#1577 = MANIFOLD_SOLID_BREP ( 'M10 Machine Threads Stud1', #754 ) ;
#1578 = ADVANCED_FACE ( 'NONE', ( #1240, #1044 ), #1250, .T. ) ;
#1579 = CARTESIAN_POINT ( 'NONE',  ( -34.00000000000000000, -25.00000000000000000, 6.000000000000000000 ) ) ;
#1580 =( NAMED_UNIT ( * ) PLANE_ANGLE_UNIT ( ) SI_UNIT ( $, .RADIAN. ) );
#1581 = ORIENTED_EDGE ( 'NONE', *, *, #920, .T. ) ;
#1582 = CARTESIAN_POINT ( 'NONE',  ( 0.000000000000000000, -2.168404344971008868E-16, 4.999999999999998224 ) ) ;
#1583 = CYLINDRICAL_SURFACE ( 'NONE', #744, 2.649999999999985700 ) ;
#1584 = CARTESIAN_POINT ( 'NONE',  ( -6.873863542433761076, -30.00000000000000000, -3.000000000000000000 ) ) ;
#1585 = ADVANCED_FACE ( 'NONE', ( #2859 ), #172, .T. ) ;
#1586 = PRODUCT ( 'Jaw Pivot Link Plate', 'Jaw Pivot Link Plate', '', ( #805 ) ) ;
#1587 = EDGE_LOOP ( 'NONE', ( #1294, #2579 ) ) ;
#1588 = CARTESIAN_POINT ( 'NONE',  ( 4.171999999999999709, -150.0000000000000000, 0.000000000000000000 ) ) ;
#1589 = DIRECTION ( 'NONE',  ( 0.8660254037844401509, 0.4999999999999971689, 1.243062518353660769E-16 ) ) ;
#1590 = VECTOR ( 'NONE', #1487, 1000.000000000000000 ) ;
#1591 = ORIENTED_EDGE ( 'NONE', *, *, #1719, .T. ) ;
#1592 = VECTOR ( 'NONE', #1650, 1000.000000000000000 ) ;
#1593 = CARTESIAN_POINT ( 'NONE',  ( -11.54700538379251107, 13.00000000000000178, 3.469741003519073858E-15 ) ) ;
#1594 =( NAMED_UNIT ( * ) PLANE_ANGLE_UNIT ( ) SI_UNIT ( $, .RADIAN. ) );
#1595 = ORIENTED_EDGE ( 'NONE', *, *, #1632, .F. ) ;
#1596 = AXIS2_PLACEMENT_3D ( 'NONE', #1241, #2150, #160 ) ;
#1597 = LINE ( 'NONE', #296, #2526 ) ;
#1598 = EDGE_CURVE ( 'NONE', #294, #2151, #2822, .T. ) ;
#1599 =( LENGTH_UNIT ( ) NAMED_UNIT ( * ) SI_UNIT ( .MILLI., .METRE. ) );
#1600 =( NAMED_UNIT ( * ) PLANE_ANGLE_UNIT ( ) SI_UNIT ( $, .RADIAN. ) );
#1601 = ORIENTED_EDGE ( 'NONE', *, *, #1965, .F. ) ;
#1602 = CARTESIAN_POINT ( 'NONE',  ( 0.000000000000000000, 0.000000000000000000, -6.000000000000000000 ) ) ;
#1603 = AXIS2_PLACEMENT_3D ( 'NONE', #1984, #2014, #1784 ) ;
#1604 = ORIENTED_EDGE ( 'NONE', *, *, #2732, .F. ) ;
#1605 = DIRECTION ( 'NONE',  ( 0.000000000000000000, -0.000000000000000000, -1.000000000000000000 ) ) ;
#1606 = PLANE ( 'NONE',  #2406 ) ;
#1607 = ORIENTED_EDGE ( 'NONE', *, *, #1598, .T. ) ;
#1608 = VECTOR ( 'NONE', #317, 1000.000000000000000 ) ;
#1609 = CARTESIAN_POINT ( 'NONE',  ( 35.00000000000000711, -24.99999999999999645, -3.000000000000000444 ) ) ;
#1610 = CIRCLE ( 'NONE', #67, 2.649999999999985700 ) ;
#1611 = EDGE_LOOP ( 'NONE', ( #1682, #1948, #184, #2392, #1977, #637 ) ) ;
#1612 = CARTESIAN_POINT ( 'NONE',  ( 36.64999999999999858, -25.00000000000000000, -3.000000000000000000 ) ) ;
#1613 = VECTOR ( 'NONE', #1318, 1000.000000000000000 ) ;
#1614 = CARTESIAN_POINT ( 'NONE',  ( -5.773502691896258199, 13.00000000000000178, -9.999999999999998224 ) ) ;
#1615 = EDGE_CURVE ( 'NONE', #1556, #327, #1555, .T. ) ;
#1616 = DIRECTION ( 'NONE',  ( 0.000000000000000000, 0.000000000000000000, 1.000000000000000000 ) ) ;
#1617 = ORIENTED_EDGE ( 'NONE', *, *, #879, .T. ) ;
#1618 = DIRECTION ( 'NONE',  ( -0.000000000000000000, -0.000000000000000000, -1.000000000000000000 ) ) ;
#1619 = PLANE ( 'NONE',  #1880 ) ;
#1620 = EDGE_LOOP ( 'NONE', ( #1488, #307 ) ) ;
#1621 = DIRECTION ( 'NONE',  ( 0.000000000000000000, -0.000000000000000000, 1.000000000000000000 ) ) ;
#1622 = EDGE_CURVE ( 'NONE', #741, #908, #586, .T. ) ;
#1623 = ADVANCED_FACE ( 'NONE', ( #1725 ), #1506, .T. ) ;
#1624 = DIRECTION ( 'NONE',  ( 0.000000000000000000, 0.000000000000000000, 1.000000000000000000 ) ) ;
#1625 = ADVANCED_FACE ( 'NONE', ( #547 ), #2366, .T. ) ;
#1626 = ORIENTED_EDGE ( 'NONE', *, *, #2343, .F. ) ;
#1627 = DIRECTION ( 'NONE',  ( 0.8660254037844379305, 0.5000000000000014433, -0.000000000000000000 ) ) ;
#1628 = PLANE ( 'NONE',  #941 ) ;
#1629 = LINE ( 'NONE', #1181, #1022 ) ;
#1630 = VERTEX_POINT ( 'NONE', #401 ) ;
#1631 = CARTESIAN_POINT ( 'NONE',  ( -34.00000000000000000, -25.00000000000000000, -3.000000000000000000 ) ) ;
#1632 = EDGE_CURVE ( 'NONE', #399, #876, #987, .T. ) ;
#1633 = ORIENTED_EDGE ( 'NONE', *, *, #1065, .F. ) ;
#1634 = DIRECTION ( 'NONE',  ( -0.000000000000000000, -0.000000000000000000, 1.000000000000000000 ) ) ;
#1635 = PRODUCT_RELATED_PRODUCT_CATEGORY ( 'part', '', ( #2766 ) ) ;
#1636 = FACE_BOUND ( 'NONE', #578, .T. ) ;
#1637 = ORIENTED_EDGE ( 'NONE', *, *, #1000, .F. ) ;
#1638 = APPLICATION_CONTEXT ( 'automotive_design' ) ;
#1639 = ORIENTED_EDGE ( 'NONE', *, *, #2915, .T. ) ;
#1640 = LINE ( 'NONE', #1144, #2454 ) ;
#1641 = EDGE_LOOP ( 'NONE', ( #714, #2345, #1793, #911 ) ) ;
#1642 = CARTESIAN_POINT ( 'NONE',  ( -59.98076211353318854, -39.99999999999994316, 3.000000000000000000 ) ) ;
#1643 = CIRCLE ( 'NONE', #1683, 5.000000000000000000 ) ;
#1644 = CARTESIAN_POINT ( 'NONE',  ( 6.123233995736764310E-16, -2.168404344971008868E-16, -4.999999999999998224 ) ) ;
#1645 = DIRECTION ( 'NONE',  ( 1.000000000000000000, 0.000000000000000000, 0.000000000000000000 ) ) ;
#1646 = CARTESIAN_POINT ( 'NONE',  ( 11.54700538379251107, 13.00000000000000178, -6.939586148520149327E-15 ) ) ;
#1647 = VECTOR ( 'NONE', #376, 1000.000000000000000 ) ;
#1648 = ORIENTED_EDGE ( 'NONE', *, *, #55, .F. ) ;
#1649 = CIRCLE ( 'NONE', #557, 8.000000000000000000 ) ;
#1650 = DIRECTION ( 'NONE',  ( -0.000000000000000000, -0.000000000000000000, 1.000000000000000000 ) ) ;
#1651 = AXIS2_PLACEMENT_3D ( 'NONE', #1769, #456, #186 ) ;
#1652 = EDGE_LOOP ( 'NONE', ( #34, #241, #677, #1322 ) ) ;
#1653 = ADVANCED_FACE ( 'NONE', ( #2494 ), #856, .F. ) ;
#1654 = CARTESIAN_POINT ( 'NONE',  ( 6.873863542433761076, -30.00000000000000000, -3.000000000000000000 ) ) ;
#1655 = DIRECTION ( 'NONE',  ( 0.000000000000000000, 0.000000000000000000, -1.000000000000000000 ) ) ;
#1656 = ORIENTED_EDGE ( 'NONE', *, *, #1560, .T. ) ;
#1657 = DIRECTION ( 'NONE',  ( -1.000000000000000000, 0.000000000000000000, 0.000000000000000000 ) ) ;
#1658 = ADVANCED_FACE ( 'NONE', ( #2695 ), #1089, .F. ) ;
#1659 = CIRCLE ( 'NONE', #613, 4.133974596215571395 ) ;
#1660 = PLANE ( 'NONE',  #650 ) ;
#1661 = LINE ( 'NONE', #2589, #784 ) ;
#1662 = DIRECTION ( 'NONE',  ( 1.000000000000000000, 0.000000000000000000, 0.000000000000000000 ) ) ;
#1663 = CIRCLE ( 'NONE', #1846, 4.999999999999997335 ) ;
#1664 = ORIENTED_EDGE ( 'NONE', *, *, #2845, .F. ) ;
#1665 = EDGE_CURVE ( 'NONE', #2627, #2914, #2513, .T. ) ;
#1666 = DIRECTION ( 'NONE',  ( 0.000000000000000000, 0.000000000000000000, -1.000000000000000000 ) ) ;
#1667 = ORIENTED_EDGE ( 'NONE', *, *, #815, .T. ) ;
#1668 = CARTESIAN_POINT ( 'NONE',  ( -49.15924597065973956, -151.4177355903189550, 3.000000000000000000 ) ) ;
#1669 = EDGE_CURVE ( 'NONE', #15, #1023, #1293, .T. ) ;
#1670 = CARTESIAN_POINT ( 'NONE',  ( -39.99999999999999289, -20.00000000000000000, -3.000000000000000000 ) ) ;
#1671 = ORIENTED_EDGE ( 'NONE', *, *, #1800, .F. ) ;
#1672 = DIRECTION ( 'NONE',  ( -1.000000000000000000, 0.000000000000000000, 1.636531581110204284E-16 ) ) ;
#1673 = DIRECTION ( 'NONE',  ( 0.000000000000000000, 0.000000000000000000, -1.000000000000000000 ) ) ;
#1674 = FACE_BOUND ( 'NONE', #2662, .T. ) ;
#1675 = VERTEX_POINT ( 'NONE', #617 ) ;
#1676 = ORIENTED_EDGE ( 'NONE', *, *, #2692, .F. ) ;
#1677 = DIRECTION ( 'NONE',  ( -0.000000000000000000, -0.000000000000000000, 1.000000000000000000 ) ) ;
#1678 = LINE ( 'NONE', #2430, #1274 ) ;
#1679 = DIRECTION ( 'NONE',  ( -0.000000000000000000, -1.000000000000000000, -0.000000000000000000 ) ) ;
#1680 = ORIENTED_EDGE ( 'NONE', *, *, #1914, .F. ) ;
#1681 = LINE ( 'NONE', #1131, #1416 ) ;
#1682 = ORIENTED_EDGE ( 'NONE', *, *, #1286, .T. ) ;
#1683 = AXIS2_PLACEMENT_3D ( 'NONE', #655, #228, #2462 ) ;
#1684 = ADVANCED_FACE ( 'NONE', ( #2450, #2466 ), #220, .T. ) ;
#1685 = DIRECTION ( 'NONE',  ( 0.000000000000000000, 0.000000000000000000, 1.000000000000000000 ) ) ;
#1686 = AXIS2_PLACEMENT_3D ( 'NONE', #486, #2389, #1448 ) ;
#1687 = EDGE_LOOP ( 'NONE', ( #2193, #57, #2712, #1823, #2155 ) ) ;
#1688 = AXIS2_PLACEMENT_3D ( 'NONE', #1005, #1907, #775 ) ;
#1689 = SHAPE_REPRESENTATION ( 'Threaded Center Forcing Screw Rod', ( #2652 ), #2217 ) ;
#1690 = DIRECTION ( 'NONE',  ( 0.000000000000000000, 0.000000000000000000, 1.000000000000000000 ) ) ;
#1691 = STYLED_ITEM ( 'NONE', ( #2753 ), #2288 ) ;
#1692 = VECTOR ( 'NONE', #891, 1000.000000000000000 ) ;
#1693 = DIRECTION ( 'NONE',  ( -1.000000000000000000, 0.000000000000000000, 0.000000000000000000 ) ) ;
#1694 =( GEOMETRIC_REPRESENTATION_CONTEXT ( 3 ) GLOBAL_UNCERTAINTY_ASSIGNED_CONTEXT ( ( #446 ) ) GLOBAL_UNIT_ASSIGNED_CONTEXT ( ( #1432, #2339, #2123 ) ) REPRESENTATION_CONTEXT ( 'NONE', 'WORKASPACE' ) );
#1695 = LINE ( 'NONE', #2855, #2501 ) ;
#1696 = ORIENTED_EDGE ( 'NONE', *, *, #129, .T. ) ;
#1697 = DIRECTION ( 'NONE',  ( -0.000000000000000000, 1.000000000000000000, -0.000000000000000000 ) ) ;
#1698 = CARTESIAN_POINT ( 'NONE',  ( 35.00000000000002132, -24.99999999999999645, 3.000000000000011990 ) ) ;
#1699 = ORIENTED_EDGE ( 'NONE', *, *, #1201, .F. ) ;
#1700 = CARTESIAN_POINT ( 'NONE',  ( -45.80724301738815285, -144.1538470861320604, 3.000000000000000000 ) ) ;
#1701 = CIRCLE ( 'NONE', #902, 5.000000000000000000 ) ;
#1702 = EDGE_CURVE ( 'NONE', #1058, #2820, #2710, .T. ) ;
#1703 = VECTOR ( 'NONE', #2338, 1000.000000000000114 ) ;
#1704 = VERTEX_POINT ( 'NONE', #443 ) ;
#1705 = AXIS2_PLACEMENT_3D ( 'NONE', #2913, #2500, #406 ) ;
#1706 = DIRECTION ( 'NONE',  ( -0.4999999999999981681, 0.8660254037844397068, -0.000000000000000000 ) ) ;
#1707 = CARTESIAN_POINT ( 'NONE',  ( -64.98076211353318854, 10.00000000000005684, 3.000000000000000000 ) ) ;
#1708 = PRODUCT_CONTEXT ( 'NONE', #2613, 'mechanical' ) ;
#1709 = DIRECTION ( 'NONE',  ( -0.000000000000000000, -1.000000000000000000, -0.000000000000000000 ) ) ;
#1710 = ORIENTED_EDGE ( 'NONE', *, *, #257, .F. ) ;
#1711 = EDGE_CURVE ( 'NONE', #2357, #1775, #1789, .T. ) ;
#1712 = CARTESIAN_POINT ( 'NONE',  ( -31.00000000000002132, -30.19615242270664268, -2.999999999999995559 ) ) ;
#1713 = CYLINDRICAL_SURFACE ( 'NONE', #1367, 2.649999999999985700 ) ;
#1714 = EDGE_CURVE ( 'NONE', #2502, #26, #1533, .T. ) ;
#1715 = EDGE_LOOP ( 'NONE', ( #1813, #1591 ) ) ;
#1716 = CARTESIAN_POINT ( 'NONE',  ( -57.33076211353320417, -39.99999999999994316, 3.000000000000000888 ) ) ;
#1717 = ORIENTED_EDGE ( 'NONE', *, *, #21, .T. ) ;
#1718 = VERTEX_POINT ( 'NONE', #2227 ) ;
#1719 = EDGE_CURVE ( 'NONE', #1332, #339, #1885, .T. ) ;
#1720 = FILL_AREA_STYLE ('',( #1300 ) ) ;
#1721 = FACE_OUTER_BOUND ( 'NONE', #222, .T. ) ;
#1722 = PRODUCT_RELATED_PRODUCT_CATEGORY ( 'part', '', ( #1535 ) ) ;
#1723 = FACE_OUTER_BOUND ( 'NONE', #679, .T. ) ;
#1724 = ORIENTED_EDGE ( 'NONE', *, *, #1266, .T. ) ;
#1725 = FACE_OUTER_BOUND ( 'NONE', #264, .T. ) ;
#1726 = DIRECTION ( 'NONE',  ( 0.000000000000000000, -1.000000000000000000, 0.000000000000000000 ) ) ;
#1727 = VERTEX_POINT ( 'NONE', #2924 ) ;
#1728 = DIRECTION ( 'NONE',  ( 1.000000000000000000, 0.000000000000000000, 0.000000000000000000 ) ) ;
#1729 = VERTEX_POINT ( 'NONE', #673 ) ;
#1730 = AXIS2_PLACEMENT_3D ( 'NONE', #493, #2353, #2544 ) ;
#1731 = FACE_OUTER_BOUND ( 'NONE', #1008, .T. ) ;
#1732 = EDGE_LOOP ( 'NONE', ( #334, #832, #1855, #1351 ) ) ;
#1733 = LINE ( 'NONE', #1750, #1379 ) ;
#1734 = CARTESIAN_POINT ( 'NONE',  ( -5.773502691896248429, 3.000000000000000000, 10.00000000000000178 ) ) ;
#1735 = AXIS2_PLACEMENT_3D ( 'NONE', #1646, #919, #298 ) ;
#1736 = ADVANCED_FACE ( 'NONE', ( #1549 ), #2241, .T. ) ;
#1737 = EDGE_LOOP ( 'NONE', ( #41, #1957, #2619, #2781 ) ) ;
#1738 = MECHANICAL_DESIGN_GEOMETRIC_PRESENTATION_REPRESENTATION (  '', ( #2222 ), #791 ) ;
#1739 = CIRCLE ( 'NONE', #747, 4.999999999999997335 ) ;
#1740 = DIRECTION ( 'NONE',  ( 0.000000000000000000, 0.000000000000000000, 1.000000000000000000 ) ) ;
#1741 = LINE ( 'NONE', #2180, #2704 ) ;
#1742 = VERTEX_POINT ( 'NONE', #230 ) ;
#1743 = LINE ( 'NONE', #839, #2523 ) ;
#1744 = ADVANCED_BREP_SHAPE_REPRESENTATION ( '', ( #1527, #2652 ), #836 ) ;
#1745 = DIRECTION ( 'NONE',  ( -0.000000000000000000, -1.000000000000000000, -0.000000000000000000 ) ) ;
#1746 = AXIS2_PLACEMENT_3D ( 'NONE', #1700, #1283, #175 ) ;
#1747 = ORIENTED_EDGE ( 'NONE', *, *, #892, .T. ) ;
#1748 = CYLINDRICAL_SURFACE ( 'NONE', #1971, 20.00000000000000355 ) ;
#1749 = EDGE_CURVE ( 'NONE', #2555, #1049, #423, .T. ) ;
#1750 = CARTESIAN_POINT ( 'NONE',  ( -45.24838417255416800, -145.5172271100825299, 3.000000000000000000 ) ) ;
#1751 = AXIS2_PLACEMENT_3D ( 'NONE', #2683, #433, #1333 ) ;
#1752 = CARTESIAN_POINT ( 'NONE',  ( -57.33076211353320417, -39.99999999999994316, -3.000000000000000444 ) ) ;
#1753 = VERTEX_POINT ( 'NONE', #2030 ) ;
#1754 = EDGE_CURVE ( 'NONE', #2644, #1806, #2665, .T. ) ;
#1755 = DIRECTION ( 'NONE',  ( 1.000000000000000000, 0.000000000000000000, 0.000000000000000000 ) ) ;
#1756 = DIRECTION ( 'NONE',  ( 0.000000000000000000, 1.000000000000000000, 0.000000000000000000 ) ) ;
#1757 = ORIENTED_EDGE ( 'NONE', *, *, #2016, .T. ) ;
#1758 = DIRECTION ( 'NONE',  ( -1.000000000000000000, 0.000000000000000000, 8.673617379884040402E-17 ) ) ;
#1759 = PLANE ( 'NONE',  #2561 ) ;
#1760 = CARTESIAN_POINT ( 'NONE',  ( -32.66987298107778059, -17.30384757729337508, 6.000000000000000000 ) ) ;
#1761 = ORIENTED_EDGE ( 'NONE', *, *, #2514, .F. ) ;
#1762 = CARTESIAN_POINT ( 'NONE',  ( -59.98076211353318854, -39.99999999999994316, 3.000000000000001332 ) ) ;
#1763 = EDGE_CURVE ( 'NONE', #1101, #2799, #383, .T. ) ;
#1764 = ORIENTED_EDGE ( 'NONE', *, *, #1264, .F. ) ;
#1765 = CARTESIAN_POINT ( 'NONE',  ( -59.98076211353318854, -39.99999999999994316, 6.000000000000000000 ) ) ;
#1766 =( NAMED_UNIT ( * ) PLANE_ANGLE_UNIT ( ) SI_UNIT ( $, .RADIAN. ) );
#1767 = CARTESIAN_POINT ( 'NONE',  ( 11.54700538379251107, 13.00000000000000178, -6.939586148520149327E-15 ) ) ;
#1768 = ORIENTED_EDGE ( 'NONE', *, *, #2845, .T. ) ;
#1769 = CARTESIAN_POINT ( 'NONE',  ( -59.98076211353318854, -39.99999999999994316, -5.999999999999996447 ) ) ;
#1770 = PRESENTATION_STYLE_ASSIGNMENT (( #1090 ) ) ;
#1771 = VERTEX_POINT ( 'NONE', #249 ) ;
#1772 = CARTESIAN_POINT ( 'NONE',  ( -64.98076211353318854, 10.00000000000005684, -3.000000000000000000 ) ) ;
#1773 = LINE ( 'NONE', #2473, #1123 ) ;
#1774 = EDGE_CURVE ( 'NONE', #2749, #1727, #1124, .T. ) ;
#1775 = VERTEX_POINT ( 'NONE', #2302 ) ;
#1776 = DIRECTION ( 'NONE',  ( -0.000000000000000000, -1.000000000000000000, -0.000000000000000000 ) ) ;
#1777 = ORIENTED_EDGE ( 'NONE', *, *, #1097, .F. ) ;
#1778 = DIRECTION ( 'NONE',  ( -0.4999999999999977796, 0.8660254037844399289, 0.000000000000000000 ) ) ;
#1779 = AXIS2_PLACEMENT_3D ( 'NONE', #544, #118, #988 ) ;
#1780 = DIRECTION ( 'NONE',  ( -1.000000000000000000, 0.000000000000000000, 0.000000000000000000 ) ) ;
#1781 = VECTOR ( 'NONE', #1706, 1000.000000000000000 ) ;
#1782 = EDGE_LOOP ( 'NONE', ( #903, #1033, #657, #1098 ) ) ;
#1783 = VECTOR ( 'NONE', #2228, 1000.000000000000000 ) ;
#1784 = DIRECTION ( 'NONE',  ( 0.000000000000000000, 0.000000000000000000, 1.000000000000000000 ) ) ;
#1785 = ORIENTED_EDGE ( 'NONE', *, *, #1174, .F. ) ;
#1786 = VECTOR ( 'NONE', #1524, 1000.000000000000000 ) ;
#1787 = DIRECTION ( 'NONE',  ( -1.000000000000000000, 0.000000000000000000, 8.673617379884040402E-17 ) ) ;
#1788 = CARTESIAN_POINT ( 'NONE',  ( -59.98076211353318854, -39.99999999999994316, 6.000000000000000000 ) ) ;
#1789 = CIRCLE ( 'NONE', #2226, 2.649999999999985700 ) ;
#1790 = CARTESIAN_POINT ( 'NONE',  ( -59.98076211353318854, -39.99999999999994316, -3.000000000000005329 ) ) ;
#1791 = EDGE_CURVE ( 'NONE', #1043, #998, #1888, .T. ) ;
#1792 = AXIS2_PLACEMENT_3D ( 'NONE', #2611, #1450, #760 ) ;
#1793 = ORIENTED_EDGE ( 'NONE', *, *, #2732, .T. ) ;
#1794 = DIRECTION ( 'NONE',  ( -0.4999999999999981681, 0.8660254037844397068, -0.000000000000000000 ) ) ;
#1795 = CARTESIAN_POINT ( 'NONE',  ( -39.99999999999999289, -20.00000000000000000, -3.000000000000000000 ) ) ;
#1796 = AXIS2_PLACEMENT_3D ( 'NONE', #234, #2530, #1408 ) ;
#1797 = VERTEX_POINT ( 'NONE', #914 ) ;
#1798 = CARTESIAN_POINT ( 'NONE',  ( 5.773502691896257311, 13.00000000000000178, -10.00000000000000000 ) ) ;
#1799 =( LENGTH_UNIT ( ) NAMED_UNIT ( * ) SI_UNIT ( .MILLI., .METRE. ) );
#1800 = EDGE_CURVE ( 'NONE', #2048, #1511, #704, .T. ) ;
#1801 = ORIENTED_EDGE ( 'NONE', *, *, #787, .F. ) ;
#1802 = CARTESIAN_POINT ( 'NONE',  ( -43.99038105676666532, -37.69615242270662492, -2.999999999999999112 ) ) ;
#1803 = PRODUCT_DEFINITION_CONTEXT ( 'detailed design', #2654, 'design' ) ;
#1804 = FACE_BOUND ( 'NONE', #1859, .T. ) ;
#1805 = CARTESIAN_POINT ( 'NONE',  ( -61.31088913245541505, -47.69615242270656807, -6.000000000000000000 ) ) ;
#1806 = VERTEX_POINT ( 'NONE', #27 ) ;
#1807 = CYLINDRICAL_SURFACE ( 'NONE', #2905, 5.000000000000000000 ) ;
#1808 = DIRECTION ( 'NONE',  ( -1.000000000000000000, 0.000000000000000000, 8.673617379884040402E-17 ) ) ;
#1809 = EDGE_CURVE ( 'NONE', #1806, #737, #2287, .T. ) ;
#1810 = VERTEX_POINT ( 'NONE', #2554 ) ;
#1811 = DIRECTION ( 'NONE',  ( 0.000000000000000000, 0.000000000000000000, 1.000000000000000000 ) ) ;
#1812 = SHAPE_REPRESENTATION_RELATIONSHIP ( 'NONE' , 'NONE' ,  #1689, #1176 ) ;
#1813 = ORIENTED_EDGE ( 'NONE', *, *, #2923, .T. ) ;
#1814 = CARTESIAN_POINT ( 'NONE',  ( -49.99038105676663690, -27.30384757729335377, 3.000000000000002665 ) ) ;
#1815 = FACE_OUTER_BOUND ( 'NONE', #1128, .T. ) ;
#1816 = CARTESIAN_POINT ( 'NONE',  ( -54.98076211353320275, 10.00000000000005684, 3.000000000000000000 ) ) ;
#1817 = CARTESIAN_POINT ( 'NONE',  ( 0.000000000000000000, -149.1719999999999970, 0.000000000000000000 ) ) ;
#1818 = VERTEX_POINT ( 'NONE', #73 ) ;
#1819 = LINE ( 'NONE', #1167, #388 ) ;
#1820 = EDGE_CURVE ( 'NONE', #15, #2634, #1406, .T. ) ;
#1821 = CARTESIAN_POINT ( 'NONE',  ( 0.000000000000000000, -1.000000000000000000, 0.000000000000000000 ) ) ;
#1822 = AXIS2_PLACEMENT_3D ( 'NONE', #333, #2870, #1223 ) ;
#1823 = ORIENTED_EDGE ( 'NONE', *, *, #920, .F. ) ;
#1824 = COLOUR_RGB ( '',0.8941176470588234615, 0.8941176470588234615, 0.8941176470588234615 ) ;
#1825 = ADVANCED_FACE ( 'NONE', ( #2074 ), #1173, .F. ) ;
#1826 = DIRECTION ( 'NONE',  ( -2.312964634635742661E-15, 0.000000000000000000, -1.000000000000000000 ) ) ;
#1827 = SURFACE_STYLE_USAGE ( .BOTH. , #40 ) ;
#1828 = VERTEX_POINT ( 'NONE', #2317 ) ;
#1829 = CIRCLE ( 'NONE', #51, 1.000000000000000000 ) ;
#1830 = LINE ( 'NONE', #2787, #2381 ) ;
#1831 = UNCERTAINTY_MEASURE_WITH_UNIT (LENGTH_MEASURE( 1.000000000000000082E-05 ), #1477, 'distance_accuracy_value', 'NONE');
#1832 = CARTESIAN_POINT ( 'NONE',  ( -64.98076211353318854, 10.00000000000005684, 3.000000000000000000 ) ) ;
#1833 = DIRECTION ( 'NONE',  ( -1.000000000000000000, 0.000000000000000000, 0.000000000000000000 ) ) ;
#1834 = CARTESIAN_POINT ( 'NONE',  ( 1.836970198721029983E-15, 3.000000000000000000, 15.00000000000000178 ) ) ;
#1835 = AXIS2_PLACEMENT_3D ( 'NONE', #1518, #413, #1755 ) ;
#1836 = ORIENTED_EDGE ( 'NONE', *, *, #783, .T. ) ;
#1837 = ADVANCED_FACE ( 'NONE', ( #719 ), #473, .F. ) ;
#1838 = CARTESIAN_POINT ( 'NONE',  ( 11.54700538379251107, 3.000000000000000000, -6.939586148520149327E-15 ) ) ;
#1839 = CIRCLE ( 'NONE', #2329, 1.000000000000000000 ) ;
#1840 = EDGE_CURVE ( 'NONE', #1871, #1842, #1271, .T. ) ;
#1841 = FACE_OUTER_BOUND ( 'NONE', #661, .T. ) ;
#1842 = VERTEX_POINT ( 'NONE', #262 ) ;
#1843 = DIRECTION ( 'NONE',  ( 0.000000000000000000, 0.000000000000000000, 1.000000000000000000 ) ) ;
#1844 = CIRCLE ( 'NONE', #299, 5.000000000000000000 ) ;
#1845 = DIRECTION ( 'NONE',  ( 0.000000000000000000, 1.000000000000000000, 0.000000000000000000 ) ) ;
#1846 = AXIS2_PLACEMENT_3D ( 'NONE', #1196, #2107, #2077 ) ;
#1847 = ORIENTED_EDGE ( 'NONE', *, *, #1097, .T. ) ;
#1848 = EDGE_CURVE ( 'NONE', #327, #1043, #292, .T. ) ;
#1849 = CARTESIAN_POINT ( 'NONE',  ( -62.63076211353317291, -39.99999999999994316, -5.999999999999996447 ) ) ;
#1850 = CIRCLE ( 'NONE', #569, 2.649999999999985700 ) ;
#1851 = LINE ( 'NONE', #1878, #1029 ) ;
#1852 = CARTESIAN_POINT ( 'NONE',  ( 0.000000000000000000, 3.000000000000000000, 0.000000000000000000 ) ) ;
#1853 = LINE ( 'NONE', #2518, #421 ) ;
#1854 = EDGE_CURVE ( 'NONE', #937, #1900, #1393, .T. ) ;
#1855 = ORIENTED_EDGE ( 'NONE', *, *, #257, .T. ) ;
#1856 = LINE ( 'NONE', #9, #19 ) ;
#1857 = CARTESIAN_POINT ( 'NONE',  ( -54.98076211353320275, 10.00000000000005684, 3.000000000000000000 ) ) ;
#1858 = ORIENTED_EDGE ( 'NONE', *, *, #2722, .T. ) ;
#1859 = EDGE_LOOP ( 'NONE', ( #702, #1143 ) ) ;
#1860 = CARTESIAN_POINT ( 'NONE',  ( 1.836970198721029983E-15, 0.000000000000000000, 15.00000000000000178 ) ) ;
#1861 = EDGE_LOOP ( 'NONE', ( #502, #1595, #2348, #1051 ) ) ;
#1862 = CARTESIAN_POINT ( 'NONE',  ( 35.00000000000001421, -30.00000000000000000, -3.000000000000000000 ) ) ;
#1863 = DIRECTION ( 'NONE',  ( 1.000000000000000000, 0.000000000000000000, -0.000000000000000000 ) ) ;
#1864 = CARTESIAN_POINT ( 'NONE',  ( 4.898587196589410857E-16, 0.000000000000000000, -3.999999999999998224 ) ) ;
#1865 = DIRECTION ( 'NONE',  ( -0.000000000000000000, 1.000000000000000000, -0.000000000000000000 ) ) ;
#1866 = EDGE_CURVE ( 'NONE', #2240, #83, #2737, .T. ) ;
#1867 = EDGE_LOOP ( 'NONE', ( #353, #1520, #2482, #1125 ) ) ;
#1868 = CARTESIAN_POINT ( 'NONE',  ( -46.49038105676664401, -33.36602540378442683, 3.000000000000002665 ) ) ;
#1869 = CARTESIAN_POINT ( 'NONE',  ( -45.24838417255416800, -145.5172271100825299, -3.000000000000000000 ) ) ;
#1870 = PRODUCT_DEFINITION_SHAPE ( 'NONE', 'NONE',  #342 ) ;
#1871 = VERTEX_POINT ( 'NONE', #1860 ) ;
#1872 = CARTESIAN_POINT ( 'NONE',  ( -64.98076211353318854, 10.00000000000005684, 3.000000000000000000 ) ) ;
#1873 = LINE ( 'NONE', #2803, #1160 ) ;
#1874 = TOROIDAL_SURFACE ( 'NONE', #1356, 4.999999999999998224, 0.9999999999999995559 ) ;
#1875 = ORIENTED_EDGE ( 'NONE', *, *, #514, .F. ) ;
#1876 = DIRECTION ( 'NONE',  ( -0.000000000000000000, -0.000000000000000000, 1.000000000000000000 ) ) ;
#1877 = AXIS2_PLACEMENT_3D ( 'NONE', #498, #1153, #2550 ) ;
#1878 = CARTESIAN_POINT ( 'NONE',  ( -39.99999999999999289, -20.00000000000000000, 3.000000000000000000 ) ) ;
#1879 = FACE_OUTER_BOUND ( 'NONE', #1898, .T. ) ;
#1880 = AXIS2_PLACEMENT_3D ( 'NONE', #511, #968, #2525 ) ;
#1881 = FACE_OUTER_BOUND ( 'NONE', #2603, .T. ) ;
#1882 = PRESENTATION_LAYER_ASSIGNMENT (  '', '', ( #1260 ) ) ;
#1883 = AXIS2_PLACEMENT_3D ( 'NONE', #649, #1557, #2716 ) ;
#1884 = VERTEX_POINT ( 'NONE', #2784 ) ;
#1885 = CIRCLE ( 'NONE', #1317, 2.649999999999985700 ) ;
#1886 = EDGE_CURVE ( 'NONE', #2357, #1332, #1640, .T. ) ;
#1887 = DIRECTION ( 'NONE',  ( 0.000000000000000000, 1.000000000000000000, 0.000000000000000000 ) ) ;
#1888 = CIRCLE ( 'NONE', #2657, 5.000000000000000888 ) ;
#1889 = ORIENTED_EDGE ( 'NONE', *, *, #111, .T. ) ;
#1890 = DIRECTION ( 'NONE',  ( -0.000000000000000000, -0.000000000000000000, -1.000000000000000000 ) ) ;
#1891 = DIRECTION ( 'NONE',  ( 1.000000000000000000, 0.000000000000000000, 0.000000000000000000 ) ) ;
#1892 = EDGE_LOOP ( 'NONE', ( #2849, #459, #2162, #1601 ) ) ;
#1893 = CARTESIAN_POINT ( 'NONE',  ( -57.33076211353320417, -69.99999999999995737, 3.000000000000000000 ) ) ;
#1894 = AXIS2_PLACEMENT_3D ( 'NONE', #468, #1618, #2537 ) ;
#1895 = PRESENTATION_STYLE_ASSIGNMENT (( #2293 ) ) ;
#1896 = DIRECTION ( 'NONE',  ( 0.000000000000000000, 0.000000000000000000, 1.000000000000000000 ) ) ;
#1897 = EDGE_CURVE ( 'NONE', #1249, #1729, #1409, .T. ) ;
#1898 = EDGE_LOOP ( 'NONE', ( #1909, #1361 ) ) ;
#1899 = CIRCLE ( 'NONE', #1939, 4.999999999999997335 ) ;
#1900 = VERTEX_POINT ( 'NONE', #2059 ) ;
#1901 = CARTESIAN_POINT ( 'NONE',  ( -5.773502691896258199, 13.00000000000000178, -9.999999999999998224 ) ) ;
#1902 = DIRECTION ( 'NONE',  ( 0.000000000000000000, -0.000000000000000000, 1.000000000000000000 ) ) ;
#1903 = FACE_BOUND ( 'NONE', #1587, .T. ) ;
#1904 = EDGE_CURVE ( 'NONE', #1753, #1810, #1544, .T. ) ;
#1905 = VERTEX_POINT ( 'NONE', #1593 ) ;
#1906 = FILL_AREA_STYLE ('',( #359 ) ) ;
#1907 = DIRECTION ( 'NONE',  ( -0.000000000000000000, 1.000000000000000000, -0.000000000000000000 ) ) ;
#1908 = ORIENTED_EDGE ( 'NONE', *, *, #2163, .T. ) ;
#1909 = ORIENTED_EDGE ( 'NONE', *, *, #142, .T. ) ;
#1910 = CARTESIAN_POINT ( 'NONE',  ( -42.16025403784441039, -30.86602540378440906, -2.999999999999997780 ) ) ;
#1911 = CARTESIAN_POINT ( 'NONE',  ( 0.000000000000000000, 3.000000000000000000, 0.000000000000000000 ) ) ;
#1912 = LINE ( 'NONE', #2837, #1590 ) ;
#1913 = ORIENTED_EDGE ( 'NONE', *, *, #671, .T. ) ;
#1914 = EDGE_CURVE ( 'NONE', #1905, #2512, #1873, .T. ) ;
#1915 = CARTESIAN_POINT ( 'NONE',  ( 35.00000000000001421, -30.00000000000000000, 3.000000000000000000 ) ) ;
#1916 = CYLINDRICAL_SURFACE ( 'NONE', #2172, 2.649999999999985700 ) ;
#1917 = EDGE_LOOP ( 'NONE', ( #2128, #858, #921, #274 ) ) ;
#1918 = CIRCLE ( 'NONE', #2168, 4.133974596215571395 ) ;
#1919 = CARTESIAN_POINT ( 'NONE',  ( 0.000000000000000000, -20.00000000000000000, 7.500000000000000888 ) ) ;
#1920 = SHAPE_REPRESENTATION_RELATIONSHIP ( 'NONE' , 'NONE' ,  #2004, #1110 ) ;
#1921 = ORIENTED_EDGE ( 'NONE', *, *, #1719, .F. ) ;
#1922 = AXIS2_PLACEMENT_3D ( 'NONE', #2208, #1756, #2680 ) ;
#1923 = CYLINDRICAL_SURFACE ( 'NONE', #2365, 5.000000000000000000 ) ;
#1924 =( GEOMETRIC_REPRESENTATION_CONTEXT ( 3 ) GLOBAL_UNCERTAINTY_ASSIGNED_CONTEXT ( ( #2740 ) ) GLOBAL_UNIT_ASSIGNED_CONTEXT ( ( #2445, #1766, #2431 ) ) REPRESENTATION_CONTEXT ( 'NONE', 'WORKASPACE' ) );
#1925 = EDGE_CURVE ( 'NONE', #2864, #2373, #328, .T. ) ;
#1926 = CIRCLE ( 'NONE', #1981, 20.00000000000000355 ) ;
#1927 = DIRECTION ( 'NONE',  ( -0.000000000000000000, -0.000000000000000000, 1.000000000000000000 ) ) ;
#1928 = EDGE_CURVE ( 'NONE', #737, #2512, #1129, .T. ) ;
#1929 = SHAPE_REPRESENTATION_RELATIONSHIP ( 'NONE' , 'NONE' ,  #1396, #2288 ) ;
#1930 = CARTESIAN_POINT ( 'NONE',  ( 5.773502691896257311, 13.00000000000000178, -10.00000000000000000 ) ) ;
#1931 = VERTEX_POINT ( 'NONE', #128 ) ;
#1932 = CARTESIAN_POINT ( 'NONE',  ( 0.000000000000000000, 0.000000000000000000, 5.000000000000000000 ) ) ;
#1933 = VECTOR ( 'NONE', #1621, 1000.000000000000000 ) ;
#1934 = CARTESIAN_POINT ( 'NONE',  ( -57.33076211353320417, -39.99999999999994316, 3.000000000000001332 ) ) ;
#1935 = EDGE_CURVE ( 'NONE', #2373, #237, #1475, .T. ) ;
#1936 = ORIENTED_EDGE ( 'NONE', *, *, #2380, .F. ) ;
#1937 = DIRECTION ( 'NONE',  ( -0.000000000000000000, -0.000000000000000000, -1.000000000000000000 ) ) ;
#1938 = VECTOR ( 'NONE', #2868, 1000.000000000000000 ) ;
#1939 = AXIS2_PLACEMENT_3D ( 'NONE', #1952, #2198, #1187 ) ;
#1940 = EDGE_CURVE ( 'NONE', #570, #1810, #584, .T. ) ;
#1941 = EDGE_CURVE ( 'NONE', #1961, #2648, #1695, .T. ) ;
#1942 = ORIENTED_EDGE ( 'NONE', *, *, #355, .T. ) ;
#1943 = EDGE_LOOP ( 'NONE', ( #1567, #2762, #598, #396 ) ) ;
#1944 = DIRECTION ( 'NONE',  ( 0.000000000000000000, 1.000000000000000000, 0.000000000000000000 ) ) ;
#1945 = VERTEX_POINT ( 'NONE', #819 ) ;
#1946 = DIRECTION ( 'NONE',  ( 1.000000000000000000, 0.000000000000000000, 0.000000000000000000 ) ) ;
#1947 = DIRECTION ( 'NONE',  ( -0.4999999999999981681, 0.8660254037844397068, -0.000000000000000000 ) ) ;
#1948 = ORIENTED_EDGE ( 'NONE', *, *, #2200, .T. ) ;
#1949 = CARTESIAN_POINT ( 'NONE',  ( 35.00000000000002132, -24.99999999999999645, 3.000000000000000000 ) ) ;
#1950 = LINE ( 'NONE', #2874, #2805 ) ;
#1951 = VERTEX_POINT ( 'NONE', #99 ) ;
#1952 = CARTESIAN_POINT ( 'NONE',  ( -46.49038105676660848, -33.36602540378440551, -2.999999999999996891 ) ) ;
#1953 =( LENGTH_UNIT ( ) NAMED_UNIT ( * ) SI_UNIT ( .MILLI., .METRE. ) );
#1954 = ORIENTED_EDGE ( 'NONE', *, *, #324, .F. ) ;
#1955 = ADVANCED_FACE ( 'NONE', ( #761 ), #2584, .T. ) ;
#1956 = LINE ( 'NONE', #2655, #1358 ) ;
#1957 = ORIENTED_EDGE ( 'NONE', *, *, #2916, .T. ) ;
#1958 = DIRECTION ( 'NONE',  ( 0.000000000000000000, 0.000000000000000000, 1.000000000000000000 ) ) ;
#1959 = PRODUCT_CONTEXT ( 'NONE', #326, 'mechanical' ) ;
#1960 = PLANE ( 'NONE',  #1020 ) ;
#1961 = VERTEX_POINT ( 'NONE', #357 ) ;
#1962 = DIRECTION ( 'NONE',  ( 1.000000000000000000, 0.000000000000000000, 0.000000000000000000 ) ) ;
#1963 = DIRECTION ( 'NONE',  ( -0.000000000000000000, -0.000000000000000000, 1.000000000000000000 ) ) ;
#1964 = EDGE_LOOP ( 'NONE', ( #130, #304, #989, #619 ) ) ;
#1965 = EDGE_CURVE ( 'NONE', #2653, #1503, #1247, .T. ) ;
#1966 = CYLINDRICAL_SURFACE ( 'NONE', #2335, 2.649999999999985700 ) ;
#1967 = EDGE_CURVE ( 'NONE', #53, #1503, #978, .T. ) ;
#1968 = AXIS2_PLACEMENT_3D ( 'NONE', #387, #440, #2026 ) ;
#1969 = DIRECTION ( 'NONE',  ( 0.5000000000000013323, -0.8660254037844379305, 0.000000000000000000 ) ) ;
#1970 = ORIENTED_EDGE ( 'NONE', *, *, #2314, .F. ) ;
#1971 = AXIS2_PLACEMENT_3D ( 'NONE', #591, #2674, #623 ) ;
#1972 = DIRECTION ( 'NONE',  ( -1.000000000000000000, 0.000000000000000000, 0.000000000000000000 ) ) ;
#1973 = AXIS2_PLACEMENT_3D ( 'NONE', #2196, #2618, #822 ) ;
#1974 = ADVANCED_FACE ( 'NONE', ( #319 ), #2161, .F. ) ;
#1975 = EDGE_LOOP ( 'NONE', ( #125, #563 ) ) ;
#1976 = CARTESIAN_POINT ( 'NONE',  ( 34.00000000000000000, -25.00000000000000000, -3.000000000000000000 ) ) ;
#1977 = ORIENTED_EDGE ( 'NONE', *, *, #1065, .T. ) ;
#1978 =( NAMED_UNIT ( * ) PLANE_ANGLE_UNIT ( ) SI_UNIT ( $, .RADIAN. ) );
#1979 =( GEOMETRIC_REPRESENTATION_CONTEXT ( 3 ) GLOBAL_UNCERTAINTY_ASSIGNED_CONTEXT ( ( #1036 ) ) GLOBAL_UNIT_ASSIGNED_CONTEXT ( ( #201, #1978, #182 ) ) REPRESENTATION_CONTEXT ( 'NONE', 'WORKASPACE' ) );
#1980 = CARTESIAN_POINT ( 'NONE',  ( -64.98076211353318854, 10.00000000000005684, 3.000000000000000000 ) ) ;
#1981 = AXIS2_PLACEMENT_3D ( 'NONE', #252, #2231, #1335 ) ;
#1982 = ORIENTED_EDGE ( 'NONE', *, *, #375, .T. ) ;
#1983 =( GEOMETRIC_REPRESENTATION_CONTEXT ( 3 ) GLOBAL_UNCERTAINTY_ASSIGNED_CONTEXT ( ( #2019 ) ) GLOBAL_UNIT_ASSIGNED_CONTEXT ( ( #1599, #266, #1225 ) ) REPRESENTATION_CONTEXT ( 'NONE', 'WORKASPACE' ) );
#1984 = CARTESIAN_POINT ( 'NONE',  ( 0.000000000000000000, -30.00000000000000000, 0.000000000000000000 ) ) ;
#1985 =( LENGTH_UNIT ( ) NAMED_UNIT ( * ) SI_UNIT ( .MILLI., .METRE. ) );
#1986 = ORIENTED_EDGE ( 'NONE', *, *, #2027, .F. ) ;
#1987 = DIRECTION ( 'NONE',  ( 0.000000000000000000, 0.000000000000000000, 1.000000000000000000 ) ) ;
#1988 = LINE ( 'NONE', #2276, #1168 ) ;
#1989 = LINE ( 'NONE', #861, #1692 ) ;
#1990 = AXIS2_PLACEMENT_3D ( 'NONE', #2706, #654, #1559 ) ;
#1991 = ORIENTED_EDGE ( 'NONE', *, *, #2594, .F. ) ;
#1992 = CIRCLE ( 'NONE', #2764, 3.999999999999998224 ) ;
#1993 = CARTESIAN_POINT ( 'NONE',  ( 35.00000000000000711, -25.00000000000000000, -3.000000000000000000 ) ) ;
#1994 = ORIENTED_EDGE ( 'NONE', *, *, #1186, .T. ) ;
#1995 = CARTESIAN_POINT ( 'NONE',  ( -51.82050807568884210, -34.13397459621553764, -2.999999999999998224 ) ) ;
#1996 = CIRCLE ( 'NONE', #1330, 2.649999999999985700 ) ;
#1997 = SHAPE_DEFINITION_REPRESENTATION ( #2906, #176 ) ;
#1998 = DIRECTION ( 'NONE',  ( 1.000000000000000000, 0.000000000000000000, 0.000000000000000000 ) ) ;
#1999 = ORIENTED_EDGE ( 'NONE', *, *, #782, .T. ) ;
#2000 = ORIENTED_EDGE ( 'NONE', *, *, #971, .T. ) ;
#2001 = ADVANCED_FACE ( 'NONE', ( #1903, #1723 ), #2361, .T. ) ;
#2002 = CARTESIAN_POINT ( 'NONE',  ( -34.00000000000000000, -25.00000000000000000, -3.000000000000000888 ) ) ;
#2003 = CARTESIAN_POINT ( 'NONE',  ( 0.000000000000000000, -30.00000000000000000, 0.000000000000000000 ) ) ;
#2004 = SHAPE_REPRESENTATION ( 'Central Crosshead Yoke Bar', ( #2652 ), #465 ) ;
#2005 = ORIENTED_EDGE ( 'NONE', *, *, #1286, .F. ) ;
#2006 = DIRECTION ( 'NONE',  ( 1.272690286469888396E-16, 7.347880794884083251E-17, 1.000000000000000000 ) ) ;
#2007 = DIRECTION ( 'NONE',  ( -0.000000000000000000, 1.000000000000000000, -0.000000000000000000 ) ) ;
#2008 = LINE ( 'NONE', #2279, #212 ) ;
#2009 = CARTESIAN_POINT ( 'NONE',  ( -57.33076211353321128, -9.999999999999943157, -3.000000000000005329 ) ) ;
#2010 = ORIENTED_EDGE ( 'NONE', *, *, #2182, .T. ) ;
#2011 = CARTESIAN_POINT ( 'NONE',  ( -64.98076211353316012, -131.3397459621555754, 3.000000000000000000 ) ) ;
#2012 = DIRECTION ( 'NONE',  ( -1.000000000000000000, -0.000000000000000000, -0.000000000000000000 ) ) ;
#2013 = ORIENTED_EDGE ( 'NONE', *, *, #624, .F. ) ;
#2014 = DIRECTION ( 'NONE',  ( 0.000000000000000000, 1.000000000000000000, 0.000000000000000000 ) ) ;
#2015 = ORIENTED_EDGE ( 'NONE', *, *, #479, .F. ) ;
#2016 = EDGE_CURVE ( 'NONE', #2441, #1704, #2377, .T. ) ;
#2017 = DIRECTION ( 'NONE',  ( -0.000000000000000000, -0.000000000000000000, 1.000000000000000000 ) ) ;
#2018 = PRODUCT_DEFINITION_CONTEXT ( 'detailed design', #1336, 'design' ) ;
#2019 = UNCERTAINTY_MEASURE_WITH_UNIT (LENGTH_MEASURE( 1.000000000000000082E-05 ), #1599, 'distance_accuracy_value', 'NONE');
#2020 = DIRECTION ( 'NONE',  ( -0.000000000000000000, -0.000000000000000000, -1.000000000000000000 ) ) ;
#2021 = ORIENTED_EDGE ( 'NONE', *, *, #634, .F. ) ;
#2022 = DIRECTION ( 'NONE',  ( -0.4999999999999981681, 0.8660254037844397068, -0.000000000000000000 ) ) ;
#2023 = EDGE_LOOP ( 'NONE', ( #2359, #1639, #1146, #2794 ) ) ;
#2024 = DIRECTION ( 'NONE',  ( 0.000000000000000000, 0.000000000000000000, 1.000000000000000000 ) ) ;
#2025 = VECTOR ( 'NONE', #771, 1000.000000000000114 ) ;
#2026 = DIRECTION ( 'NONE',  ( 1.000000000000000000, 0.000000000000000000, 0.000000000000000000 ) ) ;
#2027 = EDGE_CURVE ( 'NONE', #2644, #1425, #2818, .T. ) ;
#2028 = MECHANICAL_DESIGN_GEOMETRIC_PRESENTATION_REPRESENTATION (  '', ( #97 ), #285 ) ;
#2029 = DIRECTION ( 'NONE',  ( 1.000000000000000000, 0.000000000000000000, 1.076523719386531503E-16 ) ) ;
#2030 = CARTESIAN_POINT ( 'NONE',  ( -62.63076211353317291, -39.99999999999994316, 6.000000000000000888 ) ) ;
#2031 = DIRECTION ( 'NONE',  ( 0.000000000000000000, 0.000000000000000000, 1.000000000000000000 ) ) ;
#2032 =( GEOMETRIC_REPRESENTATION_CONTEXT ( 3 ) GLOBAL_UNCERTAINTY_ASSIGNED_CONTEXT ( ( #1334 ) ) GLOBAL_UNIT_ASSIGNED_CONTEXT ( ( #778, #2170, #1231 ) ) REPRESENTATION_CONTEXT ( 'NONE', 'WORKASPACE' ) );
#2033 = ORIENTED_EDGE ( 'NONE', *, *, #2782, .T. ) ;
#2034 = VECTOR ( 'NONE', #1150, 1000.000000000000000 ) ;
#2035 = CYLINDRICAL_SURFACE ( 'NONE', #481, 4.999999999999997335 ) ;
#2036 = CARTESIAN_POINT ( 'NONE',  ( 6.123233995736764310E-16, -1.999999999999980016, -4.999999999999998224 ) ) ;
#2037 = AXIS2_PLACEMENT_3D ( 'NONE', #901, #2271, #2434 ) ;
#2038 = EDGE_CURVE ( 'NONE', #1547, #2489, #2800, .T. ) ;
#2039 = DIRECTION ( 'NONE',  ( 0.000000000000000000, 0.000000000000000000, 1.000000000000000000 ) ) ;
#2040 = ADVANCED_FACE ( 'NONE', ( #1002 ), #806, .T. ) ;
#2041 = EDGE_LOOP ( 'NONE', ( #2551, #64, #407, #275 ) ) ;
#2042 = DIRECTION ( 'NONE',  ( -0.3420201433256743195, 0.9396926207859063185, 0.000000000000000000 ) ) ;
#2043 = DIRECTION ( 'NONE',  ( -0.8660254037844399289, -0.4999999999999978351, 0.000000000000000000 ) ) ;
#2044 = CIRCLE ( 'NONE', #851, 2.649999999999985700 ) ;
#2045 = ORIENTED_EDGE ( 'NONE', *, *, #532, .T. ) ;
#2046 = CARTESIAN_POINT ( 'NONE',  ( -5.773502691896258199, 3.000000000000000000, -9.999999999999998224 ) ) ;
#2047 = SURFACE_STYLE_FILL_AREA ( #2727 ) ;
#2048 = VERTEX_POINT ( 'NONE', #2147 ) ;
#2049 = CARTESIAN_POINT ( 'NONE',  ( -46.49038105676660848, -33.36602540378440551, 3.000000000000003109 ) ) ;
#2050 = ORIENTED_EDGE ( 'NONE', *, *, #1484, .T. ) ;
#2051 = UNCERTAINTY_MEASURE_WITH_UNIT (LENGTH_MEASURE( 1.000000000000000082E-05 ), #2879, 'distance_accuracy_value', 'NONE');
#2052 = DIRECTION ( 'NONE',  ( 0.000000000000000000, 0.000000000000000000, 1.000000000000000000 ) ) ;
#2053 = DIRECTION ( 'NONE',  ( 1.502314598737159524E-16, -0.000000000000000000, 1.000000000000000000 ) ) ;
#2054 = EDGE_LOOP ( 'NONE', ( #2769, #1764 ) ) ;
#2055 = FACE_BOUND ( 'NONE', #165, .T. ) ;
#2056 = EDGE_CURVE ( 'NONE', #300, #741, #2595, .T. ) ;
#2057 = CARTESIAN_POINT ( 'NONE',  ( -62.63076211353317291, -39.99999999999994316, 3.000000000000000000 ) ) ;
#2058 = ORIENTED_EDGE ( 'NONE', *, *, #1754, .F. ) ;
#2059 = CARTESIAN_POINT ( 'NONE',  ( -39.99999999999999289, -25.00000000000000000, -3.000000000000000000 ) ) ;
#2060 = SURFACE_STYLE_FILL_AREA ( #2511 ) ;
#2061 = ORIENTED_EDGE ( 'NONE', *, *, #2156, .T. ) ;
#2062 = FACE_OUTER_BOUND ( 'NONE', #1732, .T. ) ;
#2063 = DIRECTION ( 'NONE',  ( 0.000000000000000000, 0.000000000000000000, 1.000000000000000000 ) ) ;
#2064 = DIRECTION ( 'NONE',  ( 0.4999999999999968914, -0.8660254037844404840, 0.000000000000000000 ) ) ;
#2065 = ADVANCED_FACE ( 'NONE', ( #2612 ), #595, .T. ) ;
#2066 = ORIENTED_EDGE ( 'NONE', *, *, #1774, .F. ) ;
#2067 = CARTESIAN_POINT ( 'NONE',  ( -32.66987298107778059, -17.30384757729337508, 6.000000000000000000 ) ) ;
#2068 = DIRECTION ( 'NONE',  ( -1.000000000000000000, 0.000000000000000000, -0.000000000000000000 ) ) ;
#2069 = EDGE_CURVE ( 'NONE', #776, #2075, #1912, .T. ) ;
#2070 = VERTEX_POINT ( 'NONE', #2400 ) ;
#2071 = AXIS2_PLACEMENT_3D ( 'NONE', #867, #1100, #2415 ) ;
#2072 = ORIENTED_EDGE ( 'NONE', *, *, #2783, .F. ) ;
#2073 = VECTOR ( 'NONE', #323, 1000.000000000000000 ) ;
#2074 = FACE_OUTER_BOUND ( 'NONE', #1641, .T. ) ;
#2075 = VERTEX_POINT ( 'NONE', #1261 ) ;
#2076 = CIRCLE ( 'NONE', #1922, 7.500000000000000888 ) ;
#2077 = DIRECTION ( 'NONE',  ( 1.000000000000000000, 0.000000000000000000, 0.000000000000000000 ) ) ;
#2078 = DIRECTION ( 'NONE',  ( -0.000000000000000000, -0.000000000000000000, -1.000000000000000000 ) ) ;
#2079 = AXIS2_PLACEMENT_3D ( 'NONE', #169, #849, #2854 ) ;
#2080 = CARTESIAN_POINT ( 'NONE',  ( 5.773502691896257311, 13.00000000000000178, -10.00000000000000000 ) ) ;
#2081 = AXIS2_PLACEMENT_3D ( 'NONE', #1790, #2685, #2232 ) ;
#2082 = ORIENTED_EDGE ( 'NONE', *, *, #490, .F. ) ;
#2083 = PLANE ( 'NONE',  #1735 ) ;
#2084 = VECTOR ( 'NONE', #14, 1000.000000000000000 ) ;
#2085 = VERTEX_POINT ( 'NONE', #878 ) ;
#2086 = DIRECTION ( 'NONE',  ( 0.000000000000000000, 0.000000000000000000, -1.000000000000000000 ) ) ;
#2087 = FACE_BOUND ( 'NONE', #1306, .T. ) ;
#2088 = ORIENTED_EDGE ( 'NONE', *, *, #2117, .T. ) ;
#2089 = PLANE ( 'NONE',  #846 ) ;
#2090 = AXIS2_PLACEMENT_3D ( 'NONE', #2219, #1513, #1958 ) ;
#2091 = CARTESIAN_POINT ( 'NONE',  ( -39.99999999999999289, -25.00000000000000000, 3.000000000000000000 ) ) ;
#2092 = AXIS2_PLACEMENT_3D ( 'NONE', #2152, #824, #1047 ) ;
#2093 = VERTEX_POINT ( 'NONE', #899 ) ;
#2094 = CARTESIAN_POINT ( 'NONE',  ( -31.35000000000001563, -25.00000000000000000, 6.000000000000000888 ) ) ;
#2095 = VECTOR ( 'NONE', #2022, 1000.000000000000000 ) ;
#2096 = EDGE_CURVE ( 'NONE', #915, #766, #1340, .T. ) ;
#2097 = DIRECTION ( 'NONE',  ( 0.000000000000000000, 1.000000000000000000, 0.000000000000000000 ) ) ;
#2098 = LINE ( 'NONE', #1445, #2073 ) ;
#2099 = FACE_OUTER_BOUND ( 'NONE', #929, .T. ) ;
#2100 = ORIENTED_EDGE ( 'NONE', *, *, #1714, .F. ) ;
#2101 = DIRECTION ( 'NONE',  ( 0.000000000000000000, 0.000000000000000000, -1.000000000000000000 ) ) ;
#2102 = CARTESIAN_POINT ( 'NONE',  ( -61.31088913245541505, -47.69615242270656807, 6.000000000000000000 ) ) ;
#2103 = ORIENTED_EDGE ( 'NONE', *, *, #1155, .F. ) ;
#2104 = CARTESIAN_POINT ( 'NONE',  ( -59.98076211353319565, -9.999999999999943157, -3.000000000000005329 ) ) ;
#2105 = CARTESIAN_POINT ( 'NONE',  ( 0.000000000000000000, 3.000000000000000000, 0.000000000000000000 ) ) ;
#2106 = ORIENTED_EDGE ( 'NONE', *, *, #1711, .T. ) ;
#2107 = DIRECTION ( 'NONE',  ( 0.000000000000000000, 0.000000000000000000, 1.000000000000000000 ) ) ;
#2108 = SURFACE_STYLE_USAGE ( .BOTH. , #2320 ) ;
#2109 = FACE_OUTER_BOUND ( 'NONE', #2527, .T. ) ;
#2110 = EDGE_CURVE ( 'NONE', #1742, #741, #1291, .T. ) ;
#2111 = LINE ( 'NONE', #33, #103 ) ;
#2112 = ADVANCED_FACE ( 'NONE', ( #1304 ), #2661, .T. ) ;
#2113 = ORIENTED_EDGE ( 'NONE', *, *, #2692, .T. ) ;
#2114 = CARTESIAN_POINT ( 'NONE',  ( -36.64999999999999147, -25.00000000000000000, -5.999999999999996447 ) ) ;
#2115 = ORIENTED_EDGE ( 'NONE', *, *, #2571, .F. ) ;
#2116 = DIRECTION ( 'NONE',  ( 1.486905836551548832E-16, -1.000000000000000000, 0.000000000000000000 ) ) ;
#2117 = EDGE_CURVE ( 'NONE', #1371, #957, #1918, .T. ) ;
#2118 = DIRECTION ( 'NONE',  ( -1.272690286469888396E-16, -7.347880794884083251E-17, -1.000000000000000000 ) ) ;
#2119 = VECTOR ( 'NONE', #2605, 1000.000000000000000 ) ;
#2120 = ORIENTED_EDGE ( 'NONE', *, *, #111, .F. ) ;
#2121 = DIRECTION ( 'NONE',  ( -0.000000000000000000, 1.000000000000000000, -0.000000000000000000 ) ) ;
#2122 = AXIS2_PLACEMENT_3D ( 'NONE', #2491, #245, #1127 ) ;
#2123 =( NAMED_UNIT ( * ) SI_UNIT ( $, .STERADIAN. ) SOLID_ANGLE_UNIT ( ) );
#2124 = LINE ( 'NONE', #105, #1413 ) ;
#2125 = COLOUR_RGB ( '',0.8941176470588234615, 0.8941176470588234615, 0.8941176470588234615 ) ;
#2126 = ORIENTED_EDGE ( 'NONE', *, *, #2096, .F. ) ;
#2127 = CIRCLE ( 'NONE', #1263, 2.649999999999985700 ) ;
#2128 = ORIENTED_EDGE ( 'NONE', *, *, #1493, .F. ) ;
#2129 = AXIS2_PLACEMENT_3D ( 'NONE', #1103, #2679, #2253 ) ;
#2130 = EDGE_CURVE ( 'NONE', #2297, #2864, #2205, .T. ) ;
#2131 = LINE ( 'NONE', #2144, #599 ) ;
#2132 = ORIENTED_EDGE ( 'NONE', *, *, #199, .F. ) ;
#2133 = DIRECTION ( 'NONE',  ( 0.000000000000000000, 0.000000000000000000, -1.000000000000000000 ) ) ;
#2134 = VECTOR ( 'NONE', #958, 1000.000000000000000 ) ;
#2135 = DIRECTION ( 'NONE',  ( 0.000000000000000000, 0.000000000000000000, 1.000000000000000000 ) ) ;
#2136 = AXIS2_PLACEMENT_3D ( 'NONE', #1976, #2689, #1041 ) ;
#2137 = ORIENTED_EDGE ( 'NONE', *, *, #1967, .F. ) ;
#2138 = VECTOR ( 'NONE', #2349, 1000.000000000000000 ) ;
#2139 = FACE_OUTER_BOUND ( 'NONE', #631, .T. ) ;
#2140 = ORIENTED_EDGE ( 'NONE', *, *, #1791, .F. ) ;
#2141 = VECTOR ( 'NONE', #1685, 1000.000000000000000 ) ;
#2142 =( NAMED_UNIT ( * ) PLANE_ANGLE_UNIT ( ) SI_UNIT ( $, .RADIAN. ) );
#2143 = ORIENTED_EDGE ( 'NONE', *, *, #738, .F. ) ;
#2144 = CARTESIAN_POINT ( 'NONE',  ( 31.35000000000000853, -25.00000000000000000, -3.000000000000000000 ) ) ;
#2145 = ADVANCED_FACE ( 'NONE', ( #830 ), #1115, .T. ) ;
#2146 = CARTESIAN_POINT ( 'NONE',  ( -61.31088913245541505, -47.69615242270656807, 6.000000000000000000 ) ) ;
#2147 = CARTESIAN_POINT ( 'NONE',  ( -50.82050807568884210, -35.86602540378441972, -2.999999999999998224 ) ) ;
#2148 = EDGE_LOOP ( 'NONE', ( #1531, #467, #2187, #2010 ) ) ;
#2149 = DIRECTION ( 'NONE',  ( 0.000000000000000000, 0.000000000000000000, 1.000000000000000000 ) ) ;
#2150 = DIRECTION ( 'NONE',  ( -0.000000000000000000, -0.000000000000000000, 1.000000000000000000 ) ) ;
#2151 = VERTEX_POINT ( 'NONE', #1516 ) ;
#2152 = CARTESIAN_POINT ( 'NONE',  ( -47.49038105676660138, -31.63397459621553054, 3.000000000000003109 ) ) ;
#2153 = EDGE_CURVE ( 'NONE', #1462, #1292, #1643, .T. ) ;
#2154 = ADVANCED_FACE ( 'NONE', ( #2432 ), #1562, .T. ) ;
#2155 = ORIENTED_EDGE ( 'NONE', *, *, #1669, .F. ) ;
#2156 = EDGE_CURVE ( 'NONE', #2489, #1547, #2212, .T. ) ;
#2157 = DIRECTION ( 'NONE',  ( 0.000000000000000000, 0.000000000000000000, -1.000000000000000000 ) ) ;
#2158 = CARTESIAN_POINT ( 'NONE',  ( 0.000000000000000000, -3.999999999999900524, 0.000000000000000000 ) ) ;
#2159 = APPLICATION_PROTOCOL_DEFINITION ( 'draft international standard', 'automotive_design', 1998, #2654 ) ;
#2160 = ADVANCED_FACE ( 'NONE', ( #183 ), #10, .T. ) ;
#2161 = CYLINDRICAL_SURFACE ( 'NONE', #2744, 2.649999999999985700 ) ;
#2162 = ORIENTED_EDGE ( 'NONE', *, *, #36, .F. ) ;
#2163 = EDGE_CURVE ( 'NONE', #2668, #772, #1458, .T. ) ;
#2164 = EDGE_CURVE ( 'NONE', #2555, #2433, #670, .T. ) ;
#2165 = DIRECTION ( 'NONE',  ( 1.000000000000000000, 0.000000000000000000, -0.000000000000000000 ) ) ;
#2166 = CARTESIAN_POINT ( 'NONE',  ( -36.64999999999999147, -25.00000000000000000, 6.000000000000000000 ) ) ;
#2167 = EDGE_LOOP ( 'NONE', ( #1954, #181, #508, #1171 ) ) ;
#2168 = AXIS2_PLACEMENT_3D ( 'NONE', #428, #1113, #1545 ) ;
#2169 = DIRECTION ( 'NONE',  ( 1.000000000000000000, 0.000000000000000000, 0.000000000000000000 ) ) ;
#2170 =( NAMED_UNIT ( * ) PLANE_ANGLE_UNIT ( ) SI_UNIT ( $, .RADIAN. ) );
#2171 = VERTEX_POINT ( 'NONE', #850 ) ;
#2172 = AXIS2_PLACEMENT_3D ( 'NONE', #2887, #131, #2647 ) ;
#2173 = LINE ( 'NONE', #151, #1305 ) ;
#2174 = AXIS2_PLACEMENT_3D ( 'NONE', #1817, #1865, #1616 ) ;
#2175 = ORIENTED_EDGE ( 'NONE', *, *, #2163, .F. ) ;
#2176 = DIRECTION ( 'NONE',  ( 0.000000000000000000, 1.000000000000000000, 0.000000000000000000 ) ) ;
#2177 = AXIS2_PLACEMENT_3D ( 'NONE', #56, #517, #2334 ) ;
#2178 = CARTESIAN_POINT ( 'NONE',  ( -59.98076211353318854, -39.99999999999994316, 6.000000000000000000 ) ) ;
#2179 = VERTEX_POINT ( 'NONE', #1752 ) ;
#2180 = CARTESIAN_POINT ( 'NONE',  ( 35.00000000000002132, -30.00000000000000000, 3.000000000000011990 ) ) ;
#2181 = ORIENTED_EDGE ( 'NONE', *, *, #881, .T. ) ;
#2182 = EDGE_CURVE ( 'NONE', #862, #2326, #185, .T. ) ;
#2183 = LINE ( 'NONE', #1509, #256 ) ;
#2184 = CIRCLE ( 'NONE', #1990, 2.649999999999985700 ) ;
#2185 = FILL_AREA_STYLE ('',( #1272 ) ) ;
#2186 = VECTOR ( 'NONE', #1987, 1000.000000000000000 ) ;
#2187 = ORIENTED_EDGE ( 'NONE', *, *, #1174, .T. ) ;
#2188 = PRESENTATION_STYLE_ASSIGNMENT (( #422 ) ) ;
#2189 = EDGE_LOOP ( 'NONE', ( #984, #2926, #2278, #1019, #1994 ) ) ;
#2190 = DIRECTION ( 'NONE',  ( 0.000000000000000000, 0.000000000000000000, 1.000000000000000000 ) ) ;
#2191 = DIRECTION ( 'NONE',  ( 1.000000000000000000, 0.000000000000000000, -3.004629197474320528E-16 ) ) ;
#2192 = ADVANCED_FACE ( 'NONE', ( #1278 ), #1960, .F. ) ;
#2193 = ORIENTED_EDGE ( 'NONE', *, *, #1820, .T. ) ;
#2194 = ADVANCED_FACE ( 'NONE', ( #2446 ), #410, .F. ) ;
#2195 = CARTESIAN_POINT ( 'NONE',  ( -39.99999999999999289, -30.00000000000000000, 3.000000000000000000 ) ) ;
#2196 = CARTESIAN_POINT ( 'NONE',  ( 34.00000000000000000, -25.00000000000000000, 3.000000000000000000 ) ) ;
#2197 = EDGE_LOOP ( 'NONE', ( #250, #2673, #1570, #1604 ) ) ;
#2198 = DIRECTION ( 'NONE',  ( -1.272690286469888396E-16, -7.347880794884083251E-17, -1.000000000000000000 ) ) ;
#2199 = SURFACE_STYLE_USAGE ( .BOTH. , #2623 ) ;
#2200 = EDGE_CURVE ( 'NONE', #2839, #2644, #2921, .T. ) ;
#2201 = VERTEX_POINT ( 'NONE', #1857 ) ;
#2202 = DIRECTION ( 'NONE',  ( -0.000000000000000000, -0.000000000000000000, -1.000000000000000000 ) ) ;
#2203 = LINE ( 'NONE', #2920, #112 ) ;
#2204 = CARTESIAN_POINT ( 'NONE',  ( 0.000000000000000000, 0.000000000000000000, 0.000000000000000000 ) ) ;
#2205 = LINE ( 'NONE', #1795, #1302 ) ;
#2206 = VERTEX_POINT ( 'NONE', #2330 ) ;
#2207 = DIRECTION ( 'NONE',  ( 0.000000000000000000, -0.000000000000000000, 1.000000000000000000 ) ) ;
#2208 = CARTESIAN_POINT ( 'NONE',  ( 0.000000000000000000, -30.00000000000000000, 0.000000000000000000 ) ) ;
#2209 = ORIENTED_EDGE ( 'NONE', *, *, #1928, .T. ) ;
#2210 = CARTESIAN_POINT ( 'NONE',  ( -26.66987298107781257, -27.69615242270665689, 3.000000000000000000 ) ) ;
#2211 = DIRECTION ( 'NONE',  ( -0.000000000000000000, -1.000000000000000000, -0.000000000000000000 ) ) ;
#2212 = CIRCLE ( 'NONE', #1968, 2.649999999999985700 ) ;
#2213 = CARTESIAN_POINT ( 'NONE',  ( -37.91455138073065001, -142.8479302707733041, 3.000000000000000000 ) ) ;
#2214 = ORIENTED_EDGE ( 'NONE', *, *, #113, .T. ) ;
#2215 = CIRCLE ( 'NONE', #644, 5.000000000000000000 ) ;
#2216 = DIRECTION ( 'NONE',  ( 0.000000000000000000, 0.000000000000000000, -1.000000000000000000 ) ) ;
#2217 =( GEOMETRIC_REPRESENTATION_CONTEXT ( 3 ) GLOBAL_UNCERTAINTY_ASSIGNED_CONTEXT ( ( #310 ) ) GLOBAL_UNIT_ASSIGNED_CONTEXT ( ( #2495, #2484, #414 ) ) REPRESENTATION_CONTEXT ( 'NONE', 'WORKASPACE' ) );
#2218 = EDGE_LOOP ( 'NONE', ( #2408, #389, #527, #1262, #1441, #1676, #261 ) ) ;
#2219 = CARTESIAN_POINT ( 'NONE',  ( 0.000000000000000000, 0.000000000000000000, 0.000000000000000000 ) ) ;
#2220 = PRODUCT_DEFINITION ( 'UNKNOWN', '', #2750, #2018 ) ;
#2221 = PRODUCT_CONTEXT ( 'NONE', #1482, 'mechanical' ) ;
#2222 = STYLED_ITEM ( 'NONE', ( #124 ), #1744 ) ;
#2223 = CARTESIAN_POINT ( 'NONE',  ( -34.00000000000000000, -25.00000000000000000, 6.000000000000000000 ) ) ;
#2224 = CIRCLE ( 'NONE', #2322, 1.000000000000000000 ) ;
#2225 = VERTEX_POINT ( 'NONE', #471 ) ;
#2226 = AXIS2_PLACEMENT_3D ( 'NONE', #2711, #2904, #642 ) ;
#2227 = CARTESIAN_POINT ( 'NONE',  ( -67.31088913245542926, -37.30384757729331113, 3.000000000000000000 ) ) ;
#2228 = DIRECTION ( 'NONE',  ( -0.000000000000000000, -0.000000000000000000, 1.000000000000000000 ) ) ;
#2229 = ORIENTED_EDGE ( 'NONE', *, *, #1886, .F. ) ;
#2230 = LINE ( 'NONE', #1772, #2671 ) ;
#2231 = DIRECTION ( 'NONE',  ( 0.000000000000000000, 0.000000000000000000, -1.000000000000000000 ) ) ;
#2232 = DIRECTION ( 'NONE',  ( 1.000000000000000000, 0.000000000000000000, 0.000000000000000000 ) ) ;
#2233 = VECTOR ( 'NONE', #1346, 1000.000000000000000 ) ;
#2234 = DIRECTION ( 'NONE',  ( 0.4999999999999968914, -0.8660254037844404840, 0.000000000000000000 ) ) ;
#2235 = ORIENTED_EDGE ( 'NONE', *, *, #783, .F. ) ;
#2236 = CARTESIAN_POINT ( 'NONE',  ( -55.65063509461099045, -127.4999999999999432, 3.000000000000000000 ) ) ;
#2237 = VECTOR ( 'NONE', #225, 1000.000000000000227 ) ;
#2238 = CARTESIAN_POINT ( 'NONE',  ( -64.98076211353318854, 10.00000000000005684, -3.000000000000000000 ) ) ;
#2239 = EDGE_CURVE ( 'NONE', #1139, #1818, #69, .T. ) ;
#2240 = VERTEX_POINT ( 'NONE', #1189 ) ;
#2241 = PLANE ( 'NONE',  #58 ) ;
#2242 = ORIENTED_EDGE ( 'NONE', *, *, #1095, .T. ) ;
#2243 = DIRECTION ( 'NONE',  ( 1.000000000000000000, 0.000000000000000000, 0.000000000000000000 ) ) ;
#2244 = CYLINDRICAL_SURFACE ( 'NONE', #792, 2.649999999999985700 ) ;
#2245 = CARTESIAN_POINT ( 'NONE',  ( -67.31088913245538663, -37.30384757729328271, -6.000000000000000000 ) ) ;
#2246 = ADVANCED_FACE ( 'NONE', ( #25 ), #1606, .T. ) ;
#2247 = EDGE_CURVE ( 'NONE', #957, #2749, #260, .T. ) ;
#2248 = ORIENTED_EDGE ( 'NONE', *, *, #1055, .T. ) ;
#2249 = FACE_OUTER_BOUND ( 'NONE', #2709, .T. ) ;
#2250 = CARTESIAN_POINT ( 'NONE',  ( 0.000000000000000000, 13.00000000000000178, 0.000000000000000000 ) ) ;
#2251 = ORIENTED_EDGE ( 'NONE', *, *, #2901, .T. ) ;
#2252 = ADVANCED_FACE ( 'NONE', ( #50, #940 ), #1390, .F. ) ;
#2253 = DIRECTION ( 'NONE',  ( -0.8660254037844401509, -0.4999999999999971689, 0.000000000000000000 ) ) ;
#2254 = PRODUCT_DEFINITION_SHAPE ( 'NONE', 'NONE',  #2933 ) ;
#2255 = ORIENTED_EDGE ( 'NONE', *, *, #1266, .F. ) ;
#2256 = CARTESIAN_POINT ( 'NONE',  ( -67.31088913245538663, -37.30384757729328271, 6.000000000000000000 ) ) ;
#2257 = EDGE_CURVE ( 'NONE', #2634, #2648, #596, .T. ) ;
#2258 = UNCERTAINTY_MEASURE_WITH_UNIT (LENGTH_MEASURE( 1.000000000000000082E-05 ), #2847, 'distance_accuracy_value', 'NONE');
#2259 = DIRECTION ( 'NONE',  ( 0.000000000000000000, 0.000000000000000000, -1.000000000000000000 ) ) ;
#2260 = ORIENTED_EDGE ( 'NONE', *, *, #1138, .F. ) ;
#2261 = LINE ( 'NONE', #1805, #2237 ) ;
#2262 = VECTOR ( 'NONE', #1238, 1000.000000000000000 ) ;
#2263 = ORIENTED_EDGE ( 'NONE', *, *, #1228, .T. ) ;
#2264 = DIRECTION ( 'NONE',  ( -1.486905836551548586E-16, 1.000000000000000000, 0.000000000000000000 ) ) ;
#2265 = AXIS2_PLACEMENT_3D ( 'NONE', #918, #2808, #1161 ) ;
#2266 = DIRECTION ( 'NONE',  ( 0.000000000000000000, 0.000000000000000000, -1.000000000000000000 ) ) ;
#2267 = CIRCLE ( 'NONE', #1497, 2.649999999999985700 ) ;
#2268 = LINE ( 'NONE', #2508, #2134 ) ;
#2269 = COLOUR_RGB ( '',0.8941176470588234615, 0.8941176470588234615, 0.8941176470588234615 ) ;
#2270 = CIRCLE ( 'NONE', #54, 2.649999999999985700 ) ;
#2271 = DIRECTION ( 'NONE',  ( 0.000000000000000000, 0.000000000000000000, 1.000000000000000000 ) ) ;
#2272 = PRESENTATION_LAYER_ASSIGNMENT (  '', '', ( #833 ) ) ;
#2273 = ORIENTED_EDGE ( 'NONE', *, *, #964, .F. ) ;
#2274 = AXIS2_PLACEMENT_3D ( 'NONE', #2646, #809, #1265 ) ;
#2275 = DIRECTION ( 'NONE',  ( -0.000000000000000000, 0.000000000000000000, -1.000000000000000000 ) ) ;
#2276 = CARTESIAN_POINT ( 'NONE',  ( -26.66987298107781967, -27.69615242270666045, 6.000000000000000000 ) ) ;
#2277 = ADVANCED_FACE ( 'NONE', ( #2299 ), #1874, .F. ) ;
#2278 = ORIENTED_EDGE ( 'NONE', *, *, #191, .F. ) ;
#2279 = CARTESIAN_POINT ( 'NONE',  ( -55.65063509461099045, -127.4999999999999432, -3.000000000000000000 ) ) ;
#2280 = CIRCLE ( 'NONE', #2418, 3.999999999999999112 ) ;
#2281 = ORIENTED_EDGE ( 'NONE', *, *, #2571, .T. ) ;
#2282 = CARTESIAN_POINT ( 'NONE',  ( -59.98076211353318854, -39.99999999999994316, -5.999999999999996447 ) ) ;
#2283 = CIRCLE ( 'NONE', #2761, 2.649999999999985700 ) ;
#2284 = FACE_BOUND ( 'NONE', #1975, .T. ) ;
#2285 = AXIS2_PLACEMENT_3D ( 'NONE', #2669, #209, #1075 ) ;
#2286 = CARTESIAN_POINT ( 'NONE',  ( -32.66987298107778059, -17.30384757729337508, -6.000000000000000000 ) ) ;
#2287 = LINE ( 'NONE', #1426, #107 ) ;
#2288 = ADVANCED_BREP_SHAPE_REPRESENTATION ( '', ( #1538, #2652 ), #986 ) ;
#2289 = ADVANCED_FACE ( 'NONE', ( #1355, #728, #716, #682 ), #2506, .T. ) ;
#2290 = EDGE_LOOP ( 'NONE', ( #1014, #837 ) ) ;
#2291 = FACE_OUTER_BOUND ( 'NONE', #2429, .T. ) ;
#2292 = PRODUCT_DEFINITION_CONTEXT ( 'detailed design', #1638, 'design' ) ;
#2293 = SURFACE_STYLE_USAGE ( .BOTH. , #991 ) ;
#2294 = CARTESIAN_POINT ( 'NONE',  ( -11.54700538379251107, 3.000000000000000000, 3.469741003519073858E-15 ) ) ;
#2295 = CARTESIAN_POINT ( 'NONE',  ( -42.16025403784441039, -30.86602540378440906, 3.000000000000002220 ) ) ;
#2296 = ADVANCED_FACE ( 'NONE', ( #1374, #1841 ), #2779, .T. ) ;
#2297 = VERTEX_POINT ( 'NONE', #2748 ) ;
#2298 = CARTESIAN_POINT ( 'NONE',  ( 0.000000000000000000, 0.000000000000000000, 0.000000000000000000 ) ) ;
#2299 = FACE_OUTER_BOUND ( 'NONE', #2197, .T. ) ;
#2300 = ORIENTED_EDGE ( 'NONE', *, *, #75, .T. ) ;
#2301 = ORIENTED_EDGE ( 'NONE', *, *, #152, .F. ) ;
#2302 = CARTESIAN_POINT ( 'NONE',  ( -31.35000000000001563, -25.00000000000000000, -5.999999999999996447 ) ) ;
#2303 = ORIENTED_EDGE ( 'NONE', *, *, #2110, .F. ) ;
#2304 = LINE ( 'NONE', #2806, #2138 ) ;
#2305 = FILL_AREA_STYLE_COLOUR ( '', #1420 ) ;
#2306 = DIRECTION ( 'NONE',  ( 1.486905836551548832E-16, -1.000000000000000000, 0.000000000000000000 ) ) ;
#2307 = FACE_OUTER_BOUND ( 'NONE', #351, .T. ) ;
#2308 = ORIENTED_EDGE ( 'NONE', *, *, #4, .F. ) ;
#2309 = CARTESIAN_POINT ( 'NONE',  ( -34.99999999999999289, -20.00000000000000000, 0.000000000000000000 ) ) ;
#2310 = CARTESIAN_POINT ( 'NONE',  ( 0.000000000000000000, -2.500000000000000444, -4.133974596215571395 ) ) ;
#2311 = ORIENTED_EDGE ( 'NONE', *, *, #1342, .T. ) ;
#2312 = AXIS2_PLACEMENT_3D ( 'NONE', #533, #1440, #2347 ) ;
#2313 = ADVANCED_FACE ( 'NONE', ( #1636, #2087, #2284, #956 ), #1619, .F. ) ;
#2314 = EDGE_CURVE ( 'NONE', #83, #1384, #2889, .T. ) ;
#2315 = VERTEX_POINT ( 'NONE', #1869 ) ;
#2316 = CIRCLE ( 'NONE', #416, 2.649999999999985700 ) ;
#2317 = CARTESIAN_POINT ( 'NONE',  ( -41.49038105676660848, -33.36602540378440551, -2.999999999999997335 ) ) ;
#2318 = VERTEX_POINT ( 'NONE', #2057 ) ;
#2319 = DIRECTION ( 'NONE',  ( -0.000000000000000000, -0.000000000000000000, -1.000000000000000000 ) ) ;
#2320 = SURFACE_SIDE_STYLE ('',( #749 ) ) ;
#2321 = CARTESIAN_POINT ( 'NONE',  ( -6.873863542433761076, -30.00000000000000000, 3.000000000000000000 ) ) ;
#2322 = AXIS2_PLACEMENT_3D ( 'NONE', #2531, #1197, #709 ) ;
#2323 = DIRECTION ( 'NONE',  ( -1.000000000000000000, 0.000000000000000000, 1.502314598737159524E-16 ) ) ;
#2324 = VECTOR ( 'NONE', #869, 1000.000000000000000 ) ;
#2325 = ADVANCED_FACE ( 'NONE', ( #2798 ), #1574, .T. ) ;
#2326 = VERTEX_POINT ( 'NONE', #37 ) ;
#2327 = EDGE_LOOP ( 'NONE', ( #146, #2106 ) ) ;
#2328 = FACE_OUTER_BOUND ( 'NONE', #455, .T. ) ;
#2329 = AXIS2_PLACEMENT_3D ( 'NONE', #1156, #39, #1392 ) ;
#2330 = CARTESIAN_POINT ( 'NONE',  ( -32.66987298107778059, -17.30384757729337508, 6.000000000000000000 ) ) ;
#2331 = EDGE_LOOP ( 'NONE', ( #966, #2448, #1017, #2443 ) ) ;
#2332 = CARTESIAN_POINT ( 'NONE',  ( 0.000000000000000000, -0.9999999999999997780, 0.000000000000000000 ) ) ;
#2333 = EDGE_CURVE ( 'NONE', #1810, #1753, #2802, .T. ) ;
#2334 = DIRECTION ( 'NONE',  ( 0.000000000000000000, 0.000000000000000000, 1.000000000000000000 ) ) ;
#2335 = AXIS2_PLACEMENT_3D ( 'NONE', #2621, #1634, #2243 ) ;
#2336 = PRODUCT ( 'Threaded Center Forcing Screw Rod', 'Threaded Center Forcing Screw Rod', '', ( #1515 ) ) ;
#2337 = ORIENTED_EDGE ( 'NONE', *, *, #142, .F. ) ;
#2338 = DIRECTION ( 'NONE',  ( 0.8660254037844398178, 0.4999999999999977796, 0.000000000000000000 ) ) ;
#2339 =( NAMED_UNIT ( * ) PLANE_ANGLE_UNIT ( ) SI_UNIT ( $, .RADIAN. ) );
#2340 = CARTESIAN_POINT ( 'NONE',  ( -54.98076211353320275, 10.00000000000005684, -3.000000000000000000 ) ) ;
#2341 = CARTESIAN_POINT ( 'NONE',  ( 0.000000000000000000, -30.00000000000000000, -5.000000000000000000 ) ) ;
#2342 = ORIENTED_EDGE ( 'NONE', *, *, #1375, .F. ) ;
#2343 = EDGE_CURVE ( 'NONE', #1558, #772, #2131, .T. ) ;
#2344 = FACE_OUTER_BOUND ( 'NONE', #756, .T. ) ;
#2345 = ORIENTED_EDGE ( 'NONE', *, *, #2449, .T. ) ;
#2346 = CARTESIAN_POINT ( 'NONE',  ( -67.31088913245538663, -37.30384757729328271, 6.000000000000000000 ) ) ;
#2347 = DIRECTION ( 'NONE',  ( 0.000000000000000000, 0.000000000000000000, 1.000000000000000000 ) ) ;
#2348 = ORIENTED_EDGE ( 'NONE', *, *, #2481, .T. ) ;
#2349 = DIRECTION ( 'NONE',  ( -0.000000000000000000, -0.000000000000000000, -1.000000000000000000 ) ) ;
#2350 = APPLICATION_CONTEXT ( 'automotive_design' ) ;
#2351 = EDGE_CURVE ( 'NONE', #1806, #1905, #2835, .T. ) ;
#2352 = DIRECTION ( 'NONE',  ( 1.000000000000000000, 0.000000000000000000, 0.000000000000000000 ) ) ;
#2353 = DIRECTION ( 'NONE',  ( -1.272690286469888396E-16, -7.347880794884083251E-17, -1.000000000000000000 ) ) ;
#2354 = FACE_OUTER_BOUND ( 'NONE', #96, .T. ) ;
#2355 = PRODUCT_RELATED_PRODUCT_CATEGORY ( 'part', '', ( #2791 ) ) ;
#2356 = VECTOR ( 'NONE', #1378, 1000.000000000000000 ) ;
#2357 = VERTEX_POINT ( 'NONE', #2114 ) ;
#2358 = LINE ( 'NONE', #1236, #691 ) ;
#2359 = ORIENTED_EDGE ( 'NONE', *, *, #1622, .T. ) ;
#2360 = CARTESIAN_POINT ( 'NONE',  ( -54.98076211353318143, -128.6602540378443393, -3.000000000000000000 ) ) ;
#2361 = PLANE ( 'NONE',  #593 ) ;
#2362 = VECTOR ( 'NONE', #959, 1000.000000000000000 ) ;
#2363 = EDGE_LOOP ( 'NONE', ( #1091, #2311, #487, #2416, #1710, #2120, #378, #2733, #1105 ) ) ;
#2364 = DIRECTION ( 'NONE',  ( -0.000000000000000000, -0.000000000000000000, -1.000000000000000000 ) ) ;
#2365 = AXIS2_PLACEMENT_3D ( 'NONE', #354, #2827, #1666 ) ;
#2366 = CYLINDRICAL_SURFACE ( 'NONE', #1422, 15.00000000000000178 ) ;
#2367 = DIRECTION ( 'NONE',  ( -0.000000000000000000, 1.000000000000000000, -0.000000000000000000 ) ) ;
#2368 = AXIS2_PLACEMENT_3D ( 'NONE', #173, #1057, #2667 ) ;
#2369 = EDGE_LOOP ( 'NONE', ( #2229, #1256, #629, #1921 ) ) ;
#2370 = PRESENTATION_LAYER_ASSIGNMENT (  '', '', ( #1691 ) ) ;
#2371 = AXIS2_PLACEMENT_3D ( 'NONE', #735, #1182, #2809 ) ;
#2372 = ADVANCED_FACE ( 'NONE', ( #2344 ), #95, .F. ) ;
#2373 = VERTEX_POINT ( 'NONE', #1257 ) ;
#2374 = VECTOR ( 'NONE', #793, 1000.000000000000000 ) ;
#2375 = CARTESIAN_POINT ( 'NONE',  ( -31.35000000000001563, -25.00000000000000000, 6.000000000000000000 ) ) ;
#2376 = DIRECTION ( 'NONE',  ( -1.000000000000000000, 0.000000000000000000, 0.000000000000000000 ) ) ;
#2377 = LINE ( 'NONE', #2830, #2838 ) ;
#2378 = AXIS2_PLACEMENT_3D ( 'NONE', #451, #2086, #897 ) ;
#2379 = ORIENTED_EDGE ( 'NONE', *, *, #1034, .F. ) ;
#2380 = EDGE_CURVE ( 'NONE', #1884, #942, #114, .T. ) ;
#2381 = VECTOR ( 'NONE', #520, 1000.000000000000000 ) ;
#2382 = FACE_OUTER_BOUND ( 'NONE', #115, .T. ) ;
#2383 = ADVANCED_FACE ( 'NONE', ( #1203 ), #999, .T. ) ;
#2384 = ORIENTED_EDGE ( 'NONE', *, *, #574, .F. ) ;
#2385 = VECTOR ( 'NONE', #1745, 1000.000000000000000 ) ;
#2386 = CARTESIAN_POINT ( 'NONE',  ( 0.000000000000000000, -1.999999999999980016, 0.000000000000000000 ) ) ;
#2387 = EDGE_LOOP ( 'NONE', ( #826, #1215, #1908, #1626 ) ) ;
#2388 = ADVANCED_FACE ( 'NONE', ( #1473 ), #1923, .F. ) ;
#2389 = DIRECTION ( 'NONE',  ( -0.000000000000000000, -0.000000000000000000, 1.000000000000000000 ) ) ;
#2390 = CARTESIAN_POINT ( 'NONE',  ( -34.99999999999999289, -25.00000000000000000, -3.000000000000000000 ) ) ;
#2391 = CARTESIAN_POINT ( 'NONE',  ( -57.33076211353320417, -39.99999999999994316, 6.000000000000000000 ) ) ;
#2392 = ORIENTED_EDGE ( 'NONE', *, *, #2351, .T. ) ;
#2393 = DIRECTION ( 'NONE',  ( 0.8660254037844389297, -0.000000000000000000, 0.4999999999999996114 ) ) ;
#2394 = ORIENTED_EDGE ( 'NONE', *, *, #324, .T. ) ;
#2395 = CARTESIAN_POINT ( 'NONE',  ( -59.98076211353318854, -39.99999999999994316, 6.000000000000000000 ) ) ;
#2396 = ORIENTED_EDGE ( 'NONE', *, *, #1311, .T. ) ;
#2397 = CARTESIAN_POINT ( 'NONE',  ( 0.000000000000000000, -19.99999999999999645, -5.000000000000000000 ) ) ;
#2398 = DIRECTION ( 'NONE',  ( 0.000000000000000000, 0.000000000000000000, 1.000000000000000000 ) ) ;
#2399 = CARTESIAN_POINT ( 'NONE',  ( 0.000000000000000000, 0.000000000000000000, 0.000000000000000000 ) ) ;
#2400 = CARTESIAN_POINT ( 'NONE',  ( -58.09974666316956160, -143.2580143298517328, 3.000000000000000000 ) ) ;
#2401 = EDGE_CURVE ( 'NONE', #2824, #2179, #2267, .T. ) ;
#2402 = ORIENTED_EDGE ( 'NONE', *, *, #1484, .F. ) ;
#2403 =( NAMED_UNIT ( * ) SI_UNIT ( $, .STERADIAN. ) SOLID_ANGLE_UNIT ( ) );
#2404 = CARTESIAN_POINT ( 'NONE',  ( 0.000000000000000000, -3.999999999999900524, -5.000000000000000000 ) ) ;
#2405 = VERTEX_POINT ( 'NONE', #2397 ) ;
#2406 = AXIS2_PLACEMENT_3D ( 'NONE', #2102, #2043, #1169 ) ;
#2407 = DIRECTION ( 'NONE',  ( -0.5000000000000013323, 0.8660254037844378194, 0.000000000000000000 ) ) ;
#2408 = ORIENTED_EDGE ( 'NONE', *, *, #910, .T. ) ;
#2409 = MECHANICAL_DESIGN_GEOMETRIC_PRESENTATION_REPRESENTATION (  '', ( #1260 ), #2843 ) ;
#2410 = CARTESIAN_POINT ( 'NONE',  ( -18.00961894323348389, -42.69615242270662492, 3.000000000000000000 ) ) ;
#2411 = AXIS2_PLACEMENT_3D ( 'NONE', #435, #192, #2928 ) ;
#2412 = DIRECTION ( 'NONE',  ( 0.5000000000000013323, -0.8660254037844379305, 0.000000000000000000 ) ) ;
#2413 = APPLICATION_PROTOCOL_DEFINITION ( 'draft international standard', 'automotive_design', 1998, #326 ) ;
#2414 = AXIS2_PLACEMENT_3D ( 'NONE', #1359, #1116, #1740 ) ;
#2415 = DIRECTION ( 'NONE',  ( 1.000000000000000000, 0.000000000000000000, 0.000000000000000000 ) ) ;
#2416 = ORIENTED_EDGE ( 'NONE', *, *, #219, .F. ) ;
#2417 = EDGE_CURVE ( 'NONE', #1775, #339, #768, .T. ) ;
#2418 = AXIS2_PLACEMENT_3D ( 'NONE', #2332, #943, #1843 ) ;
#2419 = CARTESIAN_POINT ( 'NONE',  ( 6.123233995736766282E-16, -19.99999999999999645, 5.000000000000000000 ) ) ;
#2420 = ORIENTED_EDGE ( 'NONE', *, *, #540, .F. ) ;
#2421 = DIRECTION ( 'NONE',  ( 0.000000000000000000, 0.000000000000000000, 1.000000000000000000 ) ) ;
#2422 = AXIS2_PLACEMENT_3D ( 'NONE', #1253, #2650, #1480 ) ;
#2423 = FILL_AREA_STYLE ('',( #363 ) ) ;
#2424 = APPLICATION_CONTEXT ( 'automotive_design' ) ;
#2425 = AXIS2_PLACEMENT_3D ( 'NONE', #2395, #1492, #2169 ) ;
#2426 = ORIENTED_EDGE ( 'NONE', *, *, #2918, .F. ) ;
#2427 = CARTESIAN_POINT ( 'NONE',  ( 5.616230220889761452E-16, -150.0000000000000000, -4.171999999999999709 ) ) ;
#2428 = EDGE_CURVE ( 'NONE', #2492, #640, #49, .T. ) ;
#2429 = EDGE_LOOP ( 'NONE', ( #2255, #560, #177, #2736 ) ) ;
#2430 = CARTESIAN_POINT ( 'NONE',  ( -49.19086283016151384, -146.9521719906813928, 3.000000000000000000 ) ) ;
#2431 =( NAMED_UNIT ( * ) SI_UNIT ( $, .STERADIAN. ) SOLID_ANGLE_UNIT ( ) );
#2432 = FACE_OUTER_BOUND ( 'NONE', #1468, .T. ) ;
#2433 = VERTEX_POINT ( 'NONE', #541 ) ;
#2434 = DIRECTION ( 'NONE',  ( 1.000000000000000000, 0.000000000000000000, 0.000000000000000000 ) ) ;
#2435 = DIRECTION ( 'NONE',  ( 0.4999999999999993339, 0.000000000000000000, -0.8660254037844390407 ) ) ;
#2436 = ORIENTED_EDGE ( 'NONE', *, *, #1820, .F. ) ;
#2437 = CARTESIAN_POINT ( 'NONE',  ( -36.99999999999999289, -19.80384757729336087, 6.000000000000000000 ) ) ;
#2438 = CARTESIAN_POINT ( 'NONE',  ( -45.24838417255416800, -145.5172271100825299, 3.000000000000000000 ) ) ;
#2439 = EDGE_CURVE ( 'NONE', #2318, #1753, #2358, .T. ) ;
#2440 = LINE ( 'NONE', #1760, #380 ) ;
#2441 = VERTEX_POINT ( 'NONE', #1483 ) ;
#2442 = CARTESIAN_POINT ( 'NONE',  ( 0.000000000000000000, -19.99999999999999645, 0.000000000000000000 ) ) ;
#2443 = ORIENTED_EDGE ( 'NONE', *, *, #2333, .T. ) ;
#2444 = DIRECTION ( 'NONE',  ( 0.000000000000000000, 0.000000000000000000, 1.000000000000000000 ) ) ;
#2445 =( LENGTH_UNIT ( ) NAMED_UNIT ( * ) SI_UNIT ( .MILLI., .METRE. ) );
#2446 = FACE_OUTER_BOUND ( 'NONE', #2919, .T. ) ;
#2447 = PRODUCT_DEFINITION_SHAPE ( 'NONE', 'NONE',  #2934 ) ;
#2448 = ORIENTED_EDGE ( 'NONE', *, *, #1575, .F. ) ;
#2449 = EDGE_CURVE ( 'NONE', #1494, #705, #934, .T. ) ;
#2450 = FACE_BOUND ( 'NONE', #100, .T. ) ;
#2451 = ORIENTED_EDGE ( 'NONE', *, *, #293, .T. ) ;
#2452 = PLANE ( 'NONE',  #757 ) ;
#2453 = DIRECTION ( 'NONE',  ( 1.000000000000000000, 0.000000000000000000, 0.000000000000000000 ) ) ;
#2454 = VECTOR ( 'NONE', #731, 1000.000000000000000 ) ;
#2455 = CARTESIAN_POINT ( 'NONE',  ( 1.836970198721029983E-15, 3.000000000000000000, 15.00000000000000178 ) ) ;
#2456 = VECTOR ( 'NONE', #2306, 1000.000000000000000 ) ;
#2457 = EDGE_CURVE ( 'NONE', #2085, #2171, #1021, .T. ) ;
#2458 = DIRECTION ( 'NONE',  ( 0.000000000000000000, 0.000000000000000000, -1.000000000000000000 ) ) ;
#2459 = ORIENTED_EDGE ( 'NONE', *, *, #246, .T. ) ;
#2460 = FACE_OUTER_BOUND ( 'NONE', #330, .T. ) ;
#2461 = AXIS2_PLACEMENT_3D ( 'NONE', #818, #1303, #627 ) ;
#2462 = DIRECTION ( 'NONE',  ( 0.000000000000000000, 0.000000000000000000, -1.000000000000000000 ) ) ;
#2463 = CIRCLE ( 'NONE', #2081, 2.649999999999985700 ) ;
#2464 = ORIENTED_EDGE ( 'NONE', *, *, #1928, .F. ) ;
#2465 = TOROIDAL_SURFACE ( 'NONE', #701, 4.999999999999998224, 0.9999999999999995559 ) ;
#2466 = FACE_OUTER_BOUND ( 'NONE', #1219, .T. ) ;
#2467 = SURFACE_SIDE_STYLE ('',( #2047 ) ) ;
#2468 = EDGE_CURVE ( 'NONE', #1204, #1961, #344, .T. ) ;
#2469 = ORIENTED_EDGE ( 'NONE', *, *, #2470, .F. ) ;
#2470 = EDGE_CURVE ( 'NONE', #1511, #1945, #2850, .T. ) ;
#2471 = CARTESIAN_POINT ( 'NONE',  ( 31.35000000000001563, -25.00000000000000000, -3.000000000000001332 ) ) ;
#2472 = EDGE_CURVE ( 'NONE', #1675, #2636, #2173, .T. ) ;
#2473 = CARTESIAN_POINT ( 'NONE',  ( -62.63076211353317291, -39.99999999999994316, 6.000000000000000000 ) ) ;
#2474 = CARTESIAN_POINT ( 'NONE',  ( -34.00000000000000000, -25.00000000000000000, -5.999999999999996447 ) ) ;
#2475 = AXIS2_PLACEMENT_3D ( 'NONE', #2067, #2479, #2503 ) ;
#2476 = AXIS2_PLACEMENT_3D ( 'NONE', #308, #1627, #1430 ) ;
#2477 = EDGE_CURVE ( 'NONE', #1842, #1871, #885, .T. ) ;
#2478 = EDGE_LOOP ( 'NONE', ( #2143, #314 ) ) ;
#2479 = DIRECTION ( 'NONE',  ( 0.8660254037844404840, 0.4999999999999968914, -0.000000000000000000 ) ) ;
#2480 = CARTESIAN_POINT ( 'NONE',  ( -61.31088913245541505, -47.69615242270656807, 6.000000000000000000 ) ) ;
#2481 = EDGE_CURVE ( 'NONE', #399, #2179, #739, .T. ) ;
#2482 = ORIENTED_EDGE ( 'NONE', *, *, #2923, .F. ) ;
#2483 = DIRECTION ( 'NONE',  ( 0.000000000000000000, 0.000000000000000000, -1.000000000000000000 ) ) ;
#2484 =( NAMED_UNIT ( * ) PLANE_ANGLE_UNIT ( ) SI_UNIT ( $, .RADIAN. ) );
#2485 = EDGE_LOOP ( 'NONE', ( #365, #551, #382, #1481 ) ) ;
#2486 = CARTESIAN_POINT ( 'NONE',  ( -46.49038105676660848, -33.36602540378440551, 3.000000000000003109 ) ) ;
#2487 = FACE_OUTER_BOUND ( 'NONE', #2485, .T. ) ;
#2488 = CARTESIAN_POINT ( 'NONE',  ( 35.00000000000001421, -20.00000000000000000, 3.000000000000000000 ) ) ;
#2489 = VERTEX_POINT ( 'NONE', #384 ) ;
#2490 = DIRECTION ( 'NONE',  ( -0.000000000000000000, 1.000000000000000000, -0.000000000000000000 ) ) ;
#2491 = CARTESIAN_POINT ( 'NONE',  ( -45.80724301738815285, -144.1538470861320604, 3.000000000000000000 ) ) ;
#2492 = VERTEX_POINT ( 'NONE', #179 ) ;
#2493 = EDGE_CURVE ( 'NONE', #26, #2171, #1956, .T. ) ;
#2494 = FACE_OUTER_BOUND ( 'NONE', #2148, .T. ) ;
#2495 =( LENGTH_UNIT ( ) NAMED_UNIT ( * ) SI_UNIT ( .MILLI., .METRE. ) );
#2496 = ORIENTED_EDGE ( 'NONE', *, *, #769, .T. ) ;
#2497 = CARTESIAN_POINT ( 'NONE',  ( -49.15924597065973956, -151.4177355903189550, -3.000000000000000000 ) ) ;
#2498 = DIRECTION ( 'NONE',  ( 1.000000000000000000, 0.000000000000000000, 1.224646799147353207E-16 ) ) ;
#2499 = APPLICATION_CONTEXT ( 'automotive_design' ) ;
#2500 = DIRECTION ( 'NONE',  ( 0.000000000000000000, -1.000000000000000000, 0.000000000000000000 ) ) ;
#2501 = VECTOR ( 'NONE', #1947, 1000.000000000000000 ) ;
#2502 = VERTEX_POINT ( 'NONE', #816 ) ;
#2503 = DIRECTION ( 'NONE',  ( -0.4999999999999968914, 0.8660254037844404840, 0.000000000000000000 ) ) ;
#2504 = VECTOR ( 'NONE', #505, 1000.000000000000000 ) ;
#2505 = EDGE_CURVE ( 'NONE', #730, #1884, #198, .T. ) ;
#2506 = PLANE ( 'NONE',  #94 ) ;
#2507 = AXIS2_PLACEMENT_3D ( 'NONE', #1852, #2577, #537 ) ;
#2508 = CARTESIAN_POINT ( 'NONE',  ( 11.54700538379251107, 13.00000000000000178, -6.939586148520149327E-15 ) ) ;
#2509 = AXIS2_PLACEMENT_3D ( 'NONE', #1602, #724, #977 ) ;
#2510 = CARTESIAN_POINT ( 'NONE',  ( -36.99999999999999289, -19.80384757729336087, -2.999999999999995559 ) ) ;
#2511 = FILL_AREA_STYLE ('',( #1145 ) ) ;
#2512 = VERTEX_POINT ( 'NONE', #2294 ) ;
#2513 = CIRCLE ( 'NONE', #1603, 7.500000000000000888 ) ;
#2514 = EDGE_CURVE ( 'NONE', #2201, #1508, #1496, .T. ) ;
#2515 = DIRECTION ( 'NONE',  ( 1.000000000000000000, 0.000000000000000000, 0.000000000000000000 ) ) ;
#2516 = EDGE_CURVE ( 'NONE', #2315, #120, #214, .T. ) ;
#2517 = CARTESIAN_POINT ( 'NONE',  ( -50.82050807568884210, -35.86602540378441972, 3.000000000000001776 ) ) ;
#2518 = CARTESIAN_POINT ( 'NONE',  ( 11.54700538379251107, 3.000000000000000000, -6.939586148520149327E-15 ) ) ;
#2519 = CIRCLE ( 'NONE', #1226, 15.00000000000000178 ) ;
#2520 = AXIS2_PLACEMENT_3D ( 'NONE', #227, #922, #1401 ) ;
#2521 = ORIENTED_EDGE ( 'NONE', *, *, #2872, .F. ) ;
#2522 = PLANE ( 'NONE',  #1082 ) ;
#2523 = VECTOR ( 'NONE', #1295, 1000.000000000000000 ) ;
#2524 = APPLICATION_PROTOCOL_DEFINITION ( 'draft international standard', 'automotive_design', 1998, #2424 ) ;
#2525 = DIRECTION ( 'NONE',  ( -1.000000000000000000, 0.000000000000000000, -0.000000000000000000 ) ) ;
#2526 = VECTOR ( 'NONE', #477, 1000.000000000000114 ) ;
#2527 = EDGE_LOOP ( 'NONE', ( #1768, #2260, #1633, #2725 ) ) ;
#2528 = DIRECTION ( 'NONE',  ( 0.8660254037844398178, 0.4999999999999977796, 1.243062518353660769E-16 ) ) ;
#2529 = VERTEX_POINT ( 'NONE', #2009 ) ;
#2530 = DIRECTION ( 'NONE',  ( -1.076523719386531503E-16, -6.215312591768280423E-17, 1.000000000000000000 ) ) ;
#2531 = CARTESIAN_POINT ( 'NONE',  ( 6.123233995736764310E-16, -1.000000000000000000, -4.999999999999998224 ) ) ;
#2532 = CARTESIAN_POINT ( 'NONE',  ( -31.00000000000008171, -50.19615242270659650, 3.000000000000002220 ) ) ;
#2533 = FACE_BOUND ( 'NONE', #1298, .T. ) ;
#2534 = MANIFOLD_SOLID_BREP ( 'Fillet1', #2853 ) ;
#2535 = ADVANCED_FACE ( 'NONE', ( #1731 ), #395, .F. ) ;
#2536 = ORIENTED_EDGE ( 'NONE', *, *, #1121, .F. ) ;
#2537 = DIRECTION ( 'NONE',  ( -1.000000000000000000, 0.000000000000000000, 0.000000000000000000 ) ) ;
#2538 = CARTESIAN_POINT ( 'NONE',  ( -59.98076211353319565, -9.999999999999943157, 3.000000000000001332 ) ) ;
#2539 = ORIENTED_EDGE ( 'NONE', *, *, #366, .F. ) ;
#2540 = CARTESIAN_POINT ( 'NONE',  ( 36.64999999999999858, -25.00000000000000000, 3.000000000000000000 ) ) ;
#2541 = DIRECTION ( 'NONE',  ( 0.000000000000000000, 0.000000000000000000, 1.000000000000000000 ) ) ;
#2542 = ORIENTED_EDGE ( 'NONE', *, *, #796, .T. ) ;
#2543 = DIRECTION ( 'NONE',  ( 1.486905836551548832E-16, -1.000000000000000000, 0.000000000000000000 ) ) ;
#2544 = DIRECTION ( 'NONE',  ( -1.000000000000000000, 0.000000000000000000, 1.636531581110204284E-16 ) ) ;
#2545 = CARTESIAN_POINT ( 'NONE',  ( -34.00000000000000000, -25.00000000000000000, 3.000000000000000000 ) ) ;
#2546 = ORIENTED_EDGE ( 'NONE', *, *, #2901, .F. ) ;
#2547 = ORIENTED_EDGE ( 'NONE', *, *, #1615, .T. ) ;
#2548 = CYLINDRICAL_SURFACE ( 'NONE', #1746, 8.000000000000000000 ) ;
#2549 = EDGE_CURVE ( 'NONE', #2297, #1043, #331, .T. ) ;
#2550 = DIRECTION ( 'NONE',  ( 0.000000000000000000, -0.000000000000000000, 1.000000000000000000 ) ) ;
#2551 = ORIENTED_EDGE ( 'NONE', *, *, #1048, .F. ) ;
#2552 = DIRECTION ( 'NONE',  ( -1.076523719386531503E-16, -6.215312591768280423E-17, 1.000000000000000000 ) ) ;
#2553 = VECTOR ( 'NONE', #1096, 1000.000000000000000 ) ;
#2554 = CARTESIAN_POINT ( 'NONE',  ( -57.33076211353320417, -39.99999999999994316, 6.000000000000000888 ) ) ;
#2555 = VERTEX_POINT ( 'NONE', #2427 ) ;
#2556 = AXIS2_PLACEMENT_3D ( 'NONE', #1550, #1360, #870 ) ;
#2557 = CARTESIAN_POINT ( 'NONE',  ( -36.99999999999999289, -19.80384757729336087, -6.000000000000000000 ) ) ;
#2558 = PRESENTATION_STYLE_ASSIGNMENT (( #2108 ) ) ;
#2559 = CARTESIAN_POINT ( 'NONE',  ( 4.898587196589410857E-16, -1.999999999999980016, -3.999999999999998224 ) ) ;
#2560 = ADVANCED_FACE ( 'NONE', ( #2638 ), #2866, .T. ) ;
#2561 = AXIS2_PLACEMENT_3D ( 'NONE', #463, #2259, #235 ) ;
#2562 = CARTESIAN_POINT ( 'NONE',  ( 0.000000000000000000, -30.00000000000000000, -5.000000000000000000 ) ) ;
#2563=STYLED_ITEM('',(#2970),#1577);
#2564 = ORIENTED_EDGE ( 'NONE', *, *, #2682, .T. ) ;
#2565 = CARTESIAN_POINT ( 'NONE',  ( 0.000000000000000000, -30.00000000000000000, 0.000000000000000000 ) ) ;
#2566 = ADVANCED_FACE ( 'NONE', ( #2917 ), #1748, .T. ) ;
#2567 = VERTEX_POINT ( 'NONE', #1526 ) ;
#2568 = VECTOR ( 'NONE', #2528, 1000.000000000000114 ) ;
#2569 = CARTESIAN_POINT ( 'NONE',  ( -34.00000000000000000, -25.00000000000000000, 6.000000000000000000 ) ) ;
#2570 = VECTOR ( 'NONE', #938, 1000.000000000000000 ) ;
#2571 = EDGE_CURVE ( 'NONE', #2811, #2405, #2215, .T. ) ;
#2572 = DIRECTION ( 'NONE',  ( 1.000000000000000000, 0.000000000000000000, 0.000000000000000000 ) ) ;
#2573 = AXIS2_PLACEMENT_3D ( 'NONE', #1147, #1208, #1159 ) ;
#2574 = EDGE_CURVE ( 'NONE', #2820, #1058, #2316, .T. ) ;
#2575 = ORIENTED_EDGE ( 'NONE', *, *, #2200, .F. ) ;
#2576 = CARTESIAN_POINT ( 'NONE',  ( -36.99999999999999289, -19.80384757729336087, -3.000000000000000888 ) ) ;
#2577 = DIRECTION ( 'NONE',  ( 0.000000000000000000, 1.000000000000000000, 0.000000000000000000 ) ) ;
#2578 = LINE ( 'NONE', #2562, #2034 ) ;
#2579 = ORIENTED_EDGE ( 'NONE', *, *, #2602, .F. ) ;
#2580 =( REPRESENTATION_RELATIONSHIP ('NONE','NONE', #176, #2004 ) REPRESENTATION_RELATIONSHIP_WITH_TRANSFORMATION ( #452 )SHAPE_REPRESENTATION_RELATIONSHIP( ) );
#2581 = DIRECTION ( 'NONE',  ( -1.076523719386531503E-16, -6.215312591768280423E-17, 1.000000000000000000 ) ) ;
#2582 = ORIENTED_EDGE ( 'NONE', *, *, #1665, .F. ) ;
#2583 = DIRECTION ( 'NONE',  ( 0.000000000000000000, 0.000000000000000000, -1.000000000000000000 ) ) ;
#2584 = CYLINDRICAL_SURFACE ( 'NONE', #1779, 4.999999999999997335 ) ;
#2585 = ORIENTED_EDGE ( 'NONE', *, *, #607, .F. ) ;
#2586 = LINE ( 'NONE', #1893, #854 ) ;
#2587 = ADVANCED_FACE ( 'NONE', ( #32 ), #2742, .T. ) ;
#2588 = DIRECTION ( 'NONE',  ( -1.000000000000000000, 0.000000000000000000, 0.000000000000000000 ) ) ;
#2589 = CARTESIAN_POINT ( 'NONE',  ( 5.062658757011870954E-16, -2.500000000000000444, 4.133974596215571395 ) ) ;
#2590 = ORIENTED_EDGE ( 'NONE', *, *, #667, .F. ) ;
#2591 = ORIENTED_EDGE ( 'NONE', *, *, #191, .T. ) ;
#2592 = DIRECTION ( 'NONE',  ( 0.000000000000000000, -1.000000000000000000, 0.000000000000000000 ) ) ;
#2593 = LINE ( 'NONE', #345, #525 ) ;
#2594 = EDGE_CURVE ( 'NONE', #110, #1556, #1629, .T. ) ;
#2595 = LINE ( 'NONE', #1013, #736 ) ;
#2596 = AXIS2_PLACEMENT_3D ( 'NONE', #170, #2723, #1780 ) ;
#2597 = ORIENTED_EDGE ( 'NONE', *, *, #1009, .F. ) ;
#2598 = AXIS2_PLACEMENT_3D ( 'NONE', #329, #126, #983 ) ;
#2599 =( NAMED_UNIT ( * ) PLANE_ANGLE_UNIT ( ) SI_UNIT ( $, .RADIAN. ) );
#2600 = DIRECTION ( 'NONE',  ( 0.4999999999999996114, 0.000000000000000000, -0.8660254037844389297 ) ) ;
#2601 = VECTOR ( 'NONE', #2435, 1000.000000000000000 ) ;
#2602 = EDGE_CURVE ( 'NONE', #1797, #1517, #979, .T. ) ;
#2603 = EDGE_LOOP ( 'NONE', ( #1312, #442, #1404, #174 ) ) ;
#2604 = CARTESIAN_POINT ( 'NONE',  ( -49.15924597065973956, -151.4177355903189550, 3.000000000000000000 ) ) ;
#2605 = DIRECTION ( 'NONE',  ( 1.486905836551548832E-16, -1.000000000000000000, 0.000000000000000000 ) ) ;
#2606 =( NAMED_UNIT ( * ) SI_UNIT ( $, .STERADIAN. ) SOLID_ANGLE_UNIT ( ) );
#2607 = CIRCLE ( 'NONE', #894, 4.171999999999999709 ) ;
#2608 = EDGE_LOOP ( 'NONE', ( #2615, #2103, #2420, #2814, #545 ) ) ;
#2609 = VECTOR ( 'NONE', #430, 1000.000000000000000 ) ;
#2610 = DIRECTION ( 'NONE',  ( -0.000000000000000000, -0.000000000000000000, 1.000000000000000000 ) ) ;
#2611 = CARTESIAN_POINT ( 'NONE',  ( -45.80724301738815285, -144.1538470861320604, -3.000000000000000000 ) ) ;
#2612 = FACE_OUTER_BOUND ( 'NONE', #2637, .T. ) ;
#2613 = APPLICATION_CONTEXT ( 'automotive_design' ) ;
#2614 = VECTOR ( 'NONE', #638, 1000.000000000000000 ) ;
#2615 = ORIENTED_EDGE ( 'NONE', *, *, #2239, .T. ) ;
#2616 = CIRCLE ( 'NONE', #1327, 2.649999999999985700 ) ;
#2617 = DIRECTION ( 'NONE',  ( 0.000000000000000000, 0.000000000000000000, 1.000000000000000000 ) ) ;
#2618 = DIRECTION ( 'NONE',  ( 0.000000000000000000, 0.000000000000000000, 1.000000000000000000 ) ) ;
#2619 = ORIENTED_EDGE ( 'NONE', *, *, #65, .F. ) ;
#2620 = AXIS2_PLACEMENT_3D ( 'NONE', #1078, #1094, #2039 ) ;
#2621 = CARTESIAN_POINT ( 'NONE',  ( -59.98076211353318854, -69.99999999999995737, 3.000000000000000000 ) ) ;
#2622 = PRODUCT_DEFINITION_CONTEXT ( 'detailed design', #2424, 'design' ) ;
#2623 = SURFACE_SIDE_STYLE ('',( #1285 ) ) ;
#2624 = ORIENTED_EDGE ( 'NONE', *, *, #521, .F. ) ;
#2625 = EDGE_CURVE ( 'NONE', #2914, #640, #2098, .T. ) ;
#2626 = DIRECTION ( 'NONE',  ( -0.8660254037844398178, -0.4999999999999977796, 1.469576158976821827E-16 ) ) ;
#2627 = VERTEX_POINT ( 'NONE', #2321 ) ;
#2628 = LINE ( 'NONE', #1474, #2663 ) ;
#2629 = SHAPE_DEFINITION_REPRESENTATION ( #1184, #2004 ) ;
#2630 = DIRECTION ( 'NONE',  ( 0.000000000000000000, 0.000000000000000000, -1.000000000000000000 ) ) ;
#2631 = ORIENTED_EDGE ( 'NONE', *, *, #579, .F. ) ;
#2632 = DIRECTION ( 'NONE',  ( 1.000000000000000000, 0.000000000000000000, 0.000000000000000000 ) ) ;
#2633 = CARTESIAN_POINT ( 'NONE',  ( -57.33076211353320417, -39.99999999999994316, 3.000000000000000000 ) ) ;
#2634 = VERTEX_POINT ( 'NONE', #523 ) ;
#2635 = CARTESIAN_POINT ( 'NONE',  ( -64.31088913245535821, -132.4999999999999432, 3.000000000000000000 ) ) ;
#2636 = VERTEX_POINT ( 'NONE', #1433 ) ;
#2637 = EDGE_LOOP ( 'NONE', ( #1151, #518, #853, #2100 ) ) ;
#2638 = FACE_OUTER_BOUND ( 'NONE', #208, .T. ) ;
#2639 = EDGE_CURVE ( 'NONE', #2728, #53, #1398, .T. ) ;
#2640 = ORIENTED_EDGE ( 'NONE', *, *, #2468, .F. ) ;
#2641 = LINE ( 'NONE', #2236, #1938 ) ;
#2642 = DIRECTION ( 'NONE',  ( 0.000000000000000000, 0.000000000000000000, 1.000000000000000000 ) ) ;
#2643 = CARTESIAN_POINT ( 'NONE',  ( 0.000000000000000000, 3.000000000000000000, 0.000000000000000000 ) ) ;
#2644 = VERTEX_POINT ( 'NONE', #2080 ) ;
#2645 = AXIS2_PLACEMENT_3D ( 'NONE', #2765, #912, #1808 ) ;
#2646 = CARTESIAN_POINT ( 'NONE',  ( 0.000000000000000000, 0.000000000000000000, 0.000000000000000000 ) ) ;
#2647 = DIRECTION ( 'NONE',  ( 1.000000000000000000, 0.000000000000000000, 0.000000000000000000 ) ) ;
#2648 = VERTEX_POINT ( 'NONE', #751 ) ;
#2649 = VECTOR ( 'NONE', #1461, 1000.000000000000000 ) ;
#2650 = DIRECTION ( 'NONE',  ( -0.000000000000000000, -0.000000000000000000, 1.000000000000000000 ) ) ;
#2651 = EDGE_CURVE ( 'NONE', #1371, #1727, #1661, .T. ) ;
#2652 = AXIS2_PLACEMENT_3D ( 'NONE', #231, #2031, #1309 ) ;
#2653 = VERTEX_POINT ( 'NONE', #992 ) ;
#2654 = APPLICATION_CONTEXT ( 'automotive_design' ) ;
#2655 = CARTESIAN_POINT ( 'NONE',  ( -32.66987298107778059, -17.30384757729337508, -6.000000000000000000 ) ) ;
#2656 = MECHANICAL_DESIGN_GEOMETRIC_PRESENTATION_REPRESENTATION (  '', ( #1691 ), #1924 ) ;
#2657 = AXIS2_PLACEMENT_3D ( 'NONE', #1609, #1655, #276 ) ;
#2658 = ORIENTED_EDGE ( 'NONE', *, *, #1840, .F. ) ;
#2659 = DIRECTION ( 'NONE',  ( 0.000000000000000000, 0.000000000000000000, 1.000000000000000000 ) ) ;
#2660 = DIRECTION ( 'NONE',  ( 1.000000000000000000, 0.000000000000000000, 0.000000000000000000 ) ) ;
#2661 = PLANE ( 'NONE',  #882 ) ;
#2662 = EDGE_LOOP ( 'NONE', ( #2521, #2126, #1664, #2464, #1207, #1006 ) ) ;
#2663 = VECTOR ( 'NONE', #2116, 1000.000000000000000 ) ;
#2664 = ADVANCED_FACE ( 'NONE', ( #1411 ), #1210, .T. ) ;
#2665 = LINE ( 'NONE', #1798, #2084 ) ;
#2666 = VECTOR ( 'NONE', #1890, 1000.000000000000000 ) ;
#2667 = DIRECTION ( 'NONE',  ( -1.000000000000000000, 0.000000000000000000, 8.673617379884040402E-17 ) ) ;
#2668 = VERTEX_POINT ( 'NONE', #297 ) ;
#2669 = CARTESIAN_POINT ( 'NONE',  ( 34.00000000000000000, -25.00000000000000000, 3.000000000000000000 ) ) ;
#2670 = SHAPE_REPRESENTATION_RELATIONSHIP ( 'NONE' , 'NONE' ,  #470, #1744 ) ;
#2671 = VECTOR ( 'NONE', #1364, 1000.000000000000000 ) ;
#2672 = LINE ( 'NONE', #2701, #1471 ) ;
#2673 = ORIENTED_EDGE ( 'NONE', *, *, #1505, .T. ) ;
#2674 = DIRECTION ( 'NONE',  ( 0.000000000000000000, 0.000000000000000000, -1.000000000000000000 ) ) ;
#2675 = CARTESIAN_POINT ( 'NONE',  ( -34.99999999999999289, -25.00000000000000000, 3.000000000000000000 ) ) ;
#2676 = APPLICATION_PROTOCOL_DEFINITION ( 'draft international standard', 'automotive_design', 1998, #1336 ) ;
#2677 = DIRECTION ( 'NONE',  ( 1.000000000000000000, 1.486905836551548586E-16, -0.000000000000000000 ) ) ;
#2678 = ORIENTED_EDGE ( 'NONE', *, *, #2247, .T. ) ;
#2679 = DIRECTION ( 'NONE',  ( -0.4999999999999972244, 0.8660254037844402619, 0.000000000000000000 ) ) ;
#2680 = DIRECTION ( 'NONE',  ( 0.000000000000000000, 0.000000000000000000, 1.000000000000000000 ) ) ;
#2681 = ORIENTED_EDGE ( 'NONE', *, *, #2514, .T. ) ;
#2682 = EDGE_CURVE ( 'NONE', #1508, #93, #78, .T. ) ;
#2683 = CARTESIAN_POINT ( 'NONE',  ( -47.49038105676664401, -31.63397459621555186, 3.000000000000002665 ) ) ;
#2684 = CARTESIAN_POINT ( 'NONE',  ( -5.773502691896248429, 13.00000000000000178, 10.00000000000000178 ) ) ;
#2685 = DIRECTION ( 'NONE',  ( -0.000000000000000000, -0.000000000000000000, 1.000000000000000000 ) ) ;
#2686 = ORIENTED_EDGE ( 'NONE', *, *, #2468, .T. ) ;
#2687 = DIRECTION ( 'NONE',  ( 0.000000000000000000, 0.000000000000000000, -1.000000000000000000 ) ) ;
#2688 = ORIENTED_EDGE ( 'NONE', *, *, #1669, .T. ) ;
#2689 = DIRECTION ( 'NONE',  ( -0.000000000000000000, -0.000000000000000000, -1.000000000000000000 ) ) ;
#2690 = CARTESIAN_POINT ( 'NONE',  ( 0.000000000000000000, 0.000000000000000000, 0.000000000000000000 ) ) ;
#2691 = DIRECTION ( 'NONE',  ( -0.4999999999999998890, 0.000000000000000000, -0.8660254037844385966 ) ) ;
#2692 = EDGE_CURVE ( 'NONE', #349, #2151, #2124, .T. ) ;
#2693 = ORIENTED_EDGE ( 'NONE', *, *, #164, .F. ) ;
#2694 = ADVANCED_FACE ( 'NONE', ( #2109 ), #312, .F. ) ;
#2695 = FACE_OUTER_BOUND ( 'NONE', #140, .T. ) ;
#2696 = ORIENTED_EDGE ( 'NONE', *, *, #364, .T. ) ;
#2697 = CARTESIAN_POINT ( 'NONE',  ( -6.873863542433761076, -30.00000000000000000, 3.000000000000000000 ) ) ;
#2698 = DIRECTION ( 'NONE',  ( -0.000000000000000000, -0.000000000000000000, 1.000000000000000000 ) ) ;
#2699 = ADVANCED_FACE ( 'NONE', ( #1674, #1879 ), #950, .T. ) ;
#2700 = VECTOR ( 'NONE', #371, 1000.000000000000000 ) ;
#2701 = CARTESIAN_POINT ( 'NONE',  ( -31.00000000000002132, -30.19615242270664268, 3.000000000000000888 ) ) ;
#2702 = AXIS2_PLACEMENT_3D ( 'NONE', #1040, #1944, #1437 ) ;
#2703 = EDGE_CURVE ( 'NONE', #640, #415, #377, .T. ) ;
#2704 = VECTOR ( 'NONE', #573, 1000.000000000000000 ) ;
#2705 = ORIENTED_EDGE ( 'NONE', *, *, #129, .F. ) ;
#2706 = CARTESIAN_POINT ( 'NONE',  ( -34.00000000000000000, -25.00000000000000000, 6.000000000000000888 ) ) ;
#2707 = AXIS2_PLACEMENT_3D ( 'NONE', #2399, #2642, #2660 ) ;
#2708 = DIRECTION ( 'NONE',  ( 0.000000000000000000, -1.000000000000000000, 0.000000000000000000 ) ) ;
#2709 = EDGE_LOOP ( 'NONE', ( #954, #1405, #2888, #2922 ) ) ;
#2710 = CIRCLE ( 'NONE', #1835, 2.649999999999985700 ) ;
#2711 = CARTESIAN_POINT ( 'NONE',  ( -34.00000000000000000, -25.00000000000000000, -5.999999999999996447 ) ) ;
#2712 = ORIENTED_EDGE ( 'NONE', *, *, #1714, .T. ) ;
#2713 = DIRECTION ( 'NONE',  ( -0.000000000000000000, -0.000000000000000000, 1.000000000000000000 ) ) ;
#2714 = DIRECTION ( 'NONE',  ( -3.004629197474320528E-16, 0.000000000000000000, -1.000000000000000000 ) ) ;
#2715 = ORIENTED_EDGE ( 'NONE', *, *, #1412, .T. ) ;
#2716 = DIRECTION ( 'NONE',  ( 1.000000000000000000, 0.000000000000000000, 0.000000000000000000 ) ) ;
#2717 = AXIS2_PLACEMENT_3D ( 'NONE', #2569, #1221, #116 ) ;
#2718 = VECTOR ( 'NONE', #1119, 1000.000000000000114 ) ;
#2719 = ORIENTED_EDGE ( 'NONE', *, *, #68, .T. ) ;
#2720 = FACE_OUTER_BOUND ( 'NONE', #1080, .T. ) ;
#2721 = ADVANCED_FACE ( 'NONE', ( #548 ), #145, .F. ) ;
#2722 = EDGE_CURVE ( 'NONE', #2728, #2653, #1362, .T. ) ;
#2723 = DIRECTION ( 'NONE',  ( -0.000000000000000000, -0.000000000000000000, -1.000000000000000000 ) ) ;
#2724 = DIRECTION ( 'NONE',  ( -0.000000000000000000, -0.000000000000000000, 1.000000000000000000 ) ) ;
#2725 = ORIENTED_EDGE ( 'NONE', *, *, #1914, .T. ) ;
#2726 = CARTESIAN_POINT ( 'NONE',  ( 0.000000000000000000, 3.000000000000000000, 0.000000000000000000 ) ) ;
#2727 = FILL_AREA_STYLE ('',( #207 ) ) ;
#2728 = VERTEX_POINT ( 'NONE', #2559 ) ;
#2729 = CARTESIAN_POINT ( 'NONE',  ( -5.773502691896248429, 13.00000000000000178, 10.00000000000000178 ) ) ;
#2730 = FACE_OUTER_BOUND ( 'NONE', #305, .T. ) ;
#2731 = DIRECTION ( 'NONE',  ( 0.5000000000000004441, 0.000000000000000000, 0.8660254037844383745 ) ) ;
#2732 = EDGE_CURVE ( 'NONE', #705, #1503, #1829, .T. ) ;
#2733 = ORIENTED_EDGE ( 'NONE', *, *, #964, .T. ) ;
#2734 = CARTESIAN_POINT ( 'NONE',  ( -57.33076211353320417, -39.99999999999994316, -5.999999999999996447 ) ) ;
#2735 = ADVANCED_FACE ( 'NONE', ( #2759 ), #710, .F. ) ;
#2736 = ORIENTED_EDGE ( 'NONE', *, *, #2574, .T. ) ;
#2737 = LINE ( 'NONE', #501, #2362 ) ;
#2738 = EDGE_LOOP ( 'NONE', ( #450, #2175 ) ) ;
#2739 = LINE ( 'NONE', #1612, #1183 ) ;
#2740 = UNCERTAINTY_MEASURE_WITH_UNIT (LENGTH_MEASURE( 1.000000000000000082E-05 ), #2445, 'distance_accuracy_value', 'NONE');
#2741 = DIRECTION ( 'NONE',  ( -0.000000000000000000, -0.000000000000000000, 1.000000000000000000 ) ) ;
#2742 = PLANE ( 'NONE',  #2265 ) ;
#2743 = FACE_OUTER_BOUND ( 'NONE', #1279, .T. ) ;
#2744 = AXIS2_PLACEMENT_3D ( 'NONE', #2178, #1042, #1891 ) ;
#2745 = ORIENTED_EDGE ( 'NONE', *, *, #2516, .T. ) ;
#2746 = DIRECTION ( 'NONE',  ( 0.000000000000000000, -1.000000000000000000, 0.000000000000000000 ) ) ;
#2747 = VECTOR ( 'NONE', #1677, 1000.000000000000000 ) ;
#2748 = CARTESIAN_POINT ( 'NONE',  ( 35.00000000000001421, -20.00000000000000000, -3.000000000000000000 ) ) ;
#2749 = VERTEX_POINT ( 'NONE', #2404 ) ;
#2750 = PRODUCT_DEFINITION_FORMATION_WITH_SPECIFIED_SOURCE ( 'ANY', '', #2766, .NOT_KNOWN. ) ;
#2751 = VECTOR ( 'NONE', #2078, 1000.000000000000000 ) ;
#2752 = DIRECTION ( 'NONE',  ( 0.000000000000000000, 1.000000000000000000, 0.000000000000000000 ) ) ;
#2753 = PRESENTATION_STYLE_ASSIGNMENT (( #263 ) ) ;
#2754 = ORIENTED_EDGE ( 'NONE', *, *, #4, .T. ) ;
#2755 = PRESENTATION_LAYER_ASSIGNMENT (  '', '', ( #2563 ) ) ;
#2756 = DIRECTION ( 'NONE',  ( -0.000000000000000000, -0.000000000000000000, 1.000000000000000000 ) ) ;
#2757 = EDGE_CURVE ( 'NONE', #294, #15, #1467, .T. ) ;
#2758 = LINE ( 'NONE', #311, #197 ) ;
#2759 = FACE_OUTER_BOUND ( 'NONE', #1060, .T. ) ;
#2760 = DIRECTION ( 'NONE',  ( -0.4999999999999998890, 0.000000000000000000, -0.8660254037844385966 ) ) ;
#2761 = AXIS2_PLACEMENT_3D ( 'NONE', #2282, #242, #35 ) ;
#2762 = ORIENTED_EDGE ( 'NONE', *, *, #2439, .T. ) ;
#2763 = CARTESIAN_POINT ( 'NONE',  ( 6.873863542433761076, -20.00000000000000000, 3.000000000000000000 ) ) ;
#2764 = AXIS2_PLACEMENT_3D ( 'NONE', #2386, #301, #2421 ) ;
#2765 = CARTESIAN_POINT ( 'NONE',  ( -47.49038105676660138, -31.63397459621553054, -2.999999999999997335 ) ) ;
#2766 = PRODUCT ( 'MAS-182', 'MAS-182', '', ( #1959 ) ) ;
#2767 = ORIENTED_EDGE ( 'NONE', *, *, #773, .T. ) ;
#2768 = VECTOR ( 'NONE', #18, 1000.000000000000000 ) ;
#2769 = ORIENTED_EDGE ( 'NONE', *, *, #1763, .F. ) ;
#2770 = CARTESIAN_POINT ( 'NONE',  ( -50.82050807568884210, -35.86602540378441972, 3.000000000000001776 ) ) ;
#2771 = ORIENTED_EDGE ( 'NONE', *, *, #2651, .T. ) ;
#2772 = DIRECTION ( 'NONE',  ( -0.000000000000000000, -0.000000000000000000, -1.000000000000000000 ) ) ;
#2773 = DIRECTION ( 'NONE',  ( 1.000000000000000000, 0.000000000000000000, 8.673617379884040402E-17 ) ) ;
#2774 = DIRECTION ( 'NONE',  ( 0.000000000000000000, 0.000000000000000000, 1.000000000000000000 ) ) ;
#2775 = ADVANCED_FACE ( 'NONE', ( #360 ), #1500, .T. ) ;
#2776 = CARTESIAN_POINT ( 'NONE',  ( 5.773502691896257311, 3.000000000000000000, -10.00000000000000000 ) ) ;
#2777 = ORIENTED_EDGE ( 'NONE', *, *, #1451, .F. ) ;
#2778 = CARTESIAN_POINT ( 'NONE',  ( 0.000000000000000000, -2.500000000000000444, 0.000000000000000000 ) ) ;
#2779 = PLANE ( 'NONE',  #461 ) ;
#2780 = ORIENTED_EDGE ( 'NONE', *, *, #495, .F. ) ;
#2781 = ORIENTED_EDGE ( 'NONE', *, *, #2703, .F. ) ;
#2782 = EDGE_CURVE ( 'NONE', #1384, #83, #788, .T. ) ;
#2783 = EDGE_CURVE ( 'NONE', #81, #2433, #240, .T. ) ;
#2784 = CARTESIAN_POINT ( 'NONE',  ( -32.66987298107778770, -17.30384757729337508, 3.000000000000000000 ) ) ;
#2785 = EDGE_CURVE ( 'NONE', #1797, #2326, #1016, .T. ) ;
#2786 = EDGE_LOOP ( 'NONE', ( #2902, #2715, #1982, #1457 ) ) ;
#2787 = CARTESIAN_POINT ( 'NONE',  ( -39.99999999999999289, -30.00000000000000000, -3.000000000000000000 ) ) ;
#2788 = CARTESIAN_POINT ( 'NONE',  ( 6.123233995736766282E-16, -30.00000000000000000, 5.000000000000000000 ) ) ;
#2789 = CARTESIAN_POINT ( 'NONE',  ( 0.000000000000000000, -20.00000000000000000, 0.000000000000000000 ) ) ;
#2790 = PLANE ( 'NONE',  #2509 ) ;
#2791 = PRODUCT ( 'Central Crosshead Yoke Bar', 'Central Crosshead Yoke Bar', '', ( #1708 ) ) ;
#2792 = EDGE_CURVE ( 'NONE', #1630, #2820, #1478, .T. ) ;
#2793 = ADVANCED_FACE ( 'NONE', ( #2382 ), #1031, .T. ) ;
#2794 = ORIENTED_EDGE ( 'NONE', *, *, #2056, .T. ) ;
#2795 = DIRECTION ( 'NONE',  ( 0.000000000000000000, 1.000000000000000000, 0.000000000000000000 ) ) ;
#2796 = ORIENTED_EDGE ( 'NONE', *, *, #1132, .F. ) ;
#2797 = ADVANCED_FACE ( 'NONE', ( #794 ), #1916, .F. ) ;
#2798 = FACE_OUTER_BOUND ( 'NONE', #1417, .T. ) ;
#2799 = VERTEX_POINT ( 'NONE', #1227 ) ;
#2800 = CIRCLE ( 'NONE', #1822, 2.649999999999985700 ) ;
#2801 = DIRECTION ( 'NONE',  ( 1.000000000000000000, 0.000000000000000000, 0.000000000000000000 ) ) ;
#2802 = CIRCLE ( 'NONE', #1686, 2.649999999999985700 ) ;
#2803 = CARTESIAN_POINT ( 'NONE',  ( -11.54700538379251107, 13.00000000000000178, 3.469741003519073858E-15 ) ) ;
#2804 = ORIENTED_EDGE ( 'NONE', *, *, #2782, .F. ) ;
#2805 = VECTOR ( 'NONE', #1281, 1000.000000000000114 ) ;
#2806 = CARTESIAN_POINT ( 'NONE',  ( -36.64999999999999858, -25.00000000000000000, -3.000000000000000000 ) ) ;
#2807 = CARTESIAN_POINT ( 'NONE',  ( -31.35000000000001563, -25.00000000000000000, 3.000000000000000444 ) ) ;
#2808 = DIRECTION ( 'NONE',  ( -0.8660254037844397068, -0.4999999999999981681, 0.000000000000000000 ) ) ;
#2809 = DIRECTION ( 'NONE',  ( 0.000000000000000000, -0.000000000000000000, 1.000000000000000000 ) ) ;
#2810 = AXIS2_PLACEMENT_3D ( 'NONE', #2886, #686, #1624 ) ;
#2811 = VERTEX_POINT ( 'NONE', #2419 ) ;
#2812 = CIRCLE ( 'NONE', #1320, 4.999999999999997335 ) ;
#2813 = DIRECTION ( 'NONE',  ( 0.000000000000000000, 0.000000000000000000, 1.000000000000000000 ) ) ;
#2814 = ORIENTED_EDGE ( 'NONE', *, *, #2472, .F. ) ;
#2815 = EDGE_CURVE ( 'NONE', #23, #1558, #648, .T. ) ;
#2816 = DIRECTION ( 'NONE',  ( 1.076523719386531503E-16, 6.215312591768280423E-17, -1.000000000000000000 ) ) ;
#2817 = VECTOR ( 'NONE', #576, 1000.000000000000000 ) ;
#2818 = LINE ( 'NONE', #1930, #507 ) ;
#2819 = CIRCLE ( 'NONE', #2092, 4.999999999999997335 ) ;
#2820 = VERTEX_POINT ( 'NONE', #1934 ) ;
#2821 = CARTESIAN_POINT ( 'NONE',  ( 6.123233995736766282E-16, 0.000000000000000000, -5.000000000000000000 ) ) ;
#2822 = LINE ( 'NONE', #1712, #605 ) ;
#2823 = DIRECTION ( 'NONE',  ( 6.123233995737019950E-17, -0.8660254037844267172, 0.5000000000000207612 ) ) ;
#2824 = VERTEX_POINT ( 'NONE', #601 ) ;
#2825 = ORIENTED_EDGE ( 'NONE', *, *, #164, .T. ) ;
#2826 = EDGE_CURVE ( 'NONE', #998, #1556, #1741, .T. ) ;
#2827 = DIRECTION ( 'NONE',  ( -0.000000000000000000, -1.000000000000000000, -0.000000000000000000 ) ) ;
#2828 = LINE ( 'NONE', #2346, #1608 ) ;
#2829 = ADVANCED_FACE ( 'NONE', ( #810 ), #1713, .F. ) ;
#2830 = CARTESIAN_POINT ( 'NONE',  ( -34.99999999999999289, -30.00000000000000000, -3.000000000000000000 ) ) ;
#2831 = EDGE_LOOP ( 'NONE', ( #2426, #1564 ) ) ;
#2832 = DIRECTION ( 'NONE',  ( -0.000000000000000000, 1.000000000000000000, -0.000000000000000000 ) ) ;
#2833 = ORIENTED_EDGE ( 'NONE', *, *, #1423, .T. ) ;
#2834 = VERTEX_POINT ( 'NONE', #390 ) ;
#2835 = LINE ( 'NONE', #1901, #1118 ) ;
#2836 = DIRECTION ( 'NONE',  ( -0.8660254037844401509, -0.4999999999999971689, 0.000000000000000000 ) ) ;
#2837 = CARTESIAN_POINT ( 'NONE',  ( -5.773502691896248429, 13.00000000000000178, 10.00000000000000178 ) ) ;
#2838 = VECTOR ( 'NONE', #1026, 1000.000000000000000 ) ;
#2839 = VERTEX_POINT ( 'NONE', #1045 ) ;
#2840 = AXIS2_PLACEMENT_3D ( 'NONE', #2565, #1887, #2813 ) ;
#2841 = CARTESIAN_POINT ( 'NONE',  ( 31.35000000000000853, -25.00000000000000000, 3.000000000000000000 ) ) ;
#2842 = DIRECTION ( 'NONE',  ( -0.000000000000000000, -0.000000000000000000, 1.000000000000000000 ) ) ;
#2843 =( GEOMETRIC_REPRESENTATION_CONTEXT ( 3 ) GLOBAL_UNCERTAINTY_ASSIGNED_CONTEXT ( ( #1209 ) ) GLOBAL_UNIT_ASSIGNED_CONTEXT ( ( #1985, #1580, #431 ) ) REPRESENTATION_CONTEXT ( 'NONE', 'WORKASPACE' ) );
#2844 = ORIENTED_EDGE ( 'NONE', *, *, #1848, .T. ) ;
#2845 = EDGE_CURVE ( 'NONE', #2512, #915, #1950, .T. ) ;
#2846 = DIRECTION ( 'NONE',  ( 1.000000000000000000, 0.000000000000000000, 0.000000000000000000 ) ) ;
#2847 =( LENGTH_UNIT ( ) NAMED_UNIT ( * ) SI_UNIT ( .MILLI., .METRE. ) );
#2848 = AXIS2_PLACEMENT_3D ( 'NONE', #1631, #1434, #1385 ) ;
#2849 = ORIENTED_EDGE ( 'NONE', *, *, #579, .T. ) ;
#2850 = LINE ( 'NONE', #565, #1781 ) ;
#2851 = ORIENTED_EDGE ( 'NONE', *, *, #479, .T. ) ;
#2852 = CARTESIAN_POINT ( 'NONE',  ( -37.80724301738815285, -144.1538470861320604, 3.000000000000000000 ) ) ;
#2853 = CLOSED_SHELL ( 'NONE', ( #426, #1214, #1299, #449, #2383, #244, #2252, #1684, #2296, #1456, #370, #1578, #2388, #2535, #318, #2793, #562, #271, #1623 ) ) ;
#2854 = DIRECTION ( 'NONE',  ( 1.000000000000000000, 0.000000000000000000, 0.000000000000000000 ) ) ;
#2855 = CARTESIAN_POINT ( 'NONE',  ( -31.00000000000008171, -50.19615242270659650, -2.999999999999997780 ) ) ;
#2856 = VECTOR ( 'NONE', #24, 1000.000000000000000 ) ;
#2857 = ORIENTED_EDGE ( 'NONE', *, *, #1560, .F. ) ;
#2858 = AXIS2_PLACEMENT_3D ( 'NONE', #2049, #886, #1787 ) ;
#2859 = FACE_OUTER_BOUND ( 'NONE', #1892, .T. ) ;
#2860 = DIRECTION ( 'NONE',  ( 0.000000000000000000, 0.000000000000000000, 1.000000000000000000 ) ) ;
#2861 = ORIENTED_EDGE ( 'NONE', *, *, #540, .T. ) ;
#2862 = DIRECTION ( 'NONE',  ( 1.000000000000000000, 0.000000000000000000, 8.673617379884040402E-17 ) ) ;
#2863 = EDGE_CURVE ( 'NONE', #1828, #2151, #287, .T. ) ;
#2864 = VERTEX_POINT ( 'NONE', #618 ) ;
#2865 = ORIENTED_EDGE ( 'NONE', *, *, #852, .T. ) ;
#2866 = CYLINDRICAL_SURFACE ( 'NONE', #189, 4.999999999999997335 ) ;
#2867 = ORIENTED_EDGE ( 'NONE', *, *, #1472, .T. ) ;
#2868 = DIRECTION ( 'NONE',  ( 0.5000000000000013323, -0.8660254037844379305, 0.000000000000000000 ) ) ;
#2869 = APPLICATION_PROTOCOL_DEFINITION ( 'draft international standard', 'automotive_design', 1998, #1638 ) ;
#2870 = DIRECTION ( 'NONE',  ( -0.000000000000000000, -0.000000000000000000, 1.000000000000000000 ) ) ;
#2871 = ORIENTED_EDGE ( 'NONE', *, *, #2247, .F. ) ;
#2872 = EDGE_CURVE ( 'NONE', #766, #391, #122, .T. ) ;
#2873 = DIRECTION ( 'NONE',  ( 0.000000000000000000, 0.000000000000000000, 1.000000000000000000 ) ) ;
#2874 = CARTESIAN_POINT ( 'NONE',  ( -11.54700538379251107, 3.000000000000000000, 3.469741003519073858E-15 ) ) ;
#2875 = ORIENTED_EDGE ( 'NONE', *, *, #1472, .F. ) ;
#2876 = DIRECTION ( 'NONE',  ( -1.000000000000000000, 0.000000000000000000, 0.000000000000000000 ) ) ;
#2877 =( NAMED_UNIT ( * ) PLANE_ANGLE_UNIT ( ) SI_UNIT ( $, .RADIAN. ) );
#2878 = ORIENTED_EDGE ( 'NONE', *, *, #2130, .F. ) ;
#2879 =( LENGTH_UNIT ( ) NAMED_UNIT ( * ) SI_UNIT ( .MILLI., .METRE. ) );
#2880 = DIRECTION ( 'NONE',  ( 0.000000000000000000, 1.000000000000000000, 0.000000000000000000 ) ) ;
#2881 = ADVANCED_FACE ( 'NONE', ( #2139 ), #1069, .T. ) ;
#2882 = APPLICATION_PROTOCOL_DEFINITION ( 'draft international standard', 'automotive_design', 1998, #2350 ) ;
#2883 = DIRECTION ( 'NONE',  ( -0.8660254037844399289, -0.4999999999999978351, 0.000000000000000000 ) ) ;
#2884 = ORIENTED_EDGE ( 'NONE', *, *, #2457, .T. ) ;
#2885 = AXIS2_PLACEMENT_3D ( 'NONE', #2105, #2752, #1811 ) ;
#2886 = CARTESIAN_POINT ( 'NONE',  ( 0.000000000000000000, -3.999999999999900524, 0.000000000000000000 ) ) ;
#2887 = CARTESIAN_POINT ( 'NONE',  ( -59.98076211353318854, -39.99999999999994316, 3.000000000000000000 ) ) ;
#2888 = ORIENTED_EDGE ( 'NONE', *, *, #219, .T. ) ;
#2889 = CIRCLE ( 'NONE', #510, 2.649999999999985700 ) ;
#2890 = CARTESIAN_POINT ( 'NONE',  ( 0.000000000000000000, -19.99999999999999645, 0.000000000000000000 ) ) ;
#2891 = AXIS2_PLACEMENT_3D ( 'NONE', #1614, #2393, #2600 ) ;
#2892 = LINE ( 'NONE', #621, #1786 ) ;
#2893 = ORIENTED_EDGE ( 'NONE', *, *, #881, .F. ) ;
#2894 = DIRECTION ( 'NONE',  ( -0.000000000000000000, -0.000000000000000000, -1.000000000000000000 ) ) ;
#2895 = CARTESIAN_POINT ( 'NONE',  ( -46.49038105676664401, -33.36602540378442683, -2.999999999999998224 ) ) ;
#2896 = AXIS2_PLACEMENT_3D ( 'NONE', #765, #1673, #2588 ) ;
#2897 = ORIENTED_EDGE ( 'NONE', *, *, #2916, .F. ) ;
#2898 = LINE ( 'NONE', #1995, #2614 ) ;
#2899 = DIRECTION ( 'NONE',  ( 1.000000000000000000, 0.000000000000000000, 0.000000000000000000 ) ) ;
#2900 = DIRECTION ( 'NONE',  ( 0.000000000000000000, 0.000000000000000000, -1.000000000000000000 ) ) ;
#2901 = EDGE_CURVE ( 'NONE', #2048, #2225, #1681, .T. ) ;
#2902 = ORIENTED_EDGE ( 'NONE', *, *, #2722, .F. ) ;
#2903 = VECTOR ( 'NONE', #1927, 1000.000000000000000 ) ;
#2904 = DIRECTION ( 'NONE',  ( -0.000000000000000000, -0.000000000000000000, 1.000000000000000000 ) ) ;
#2905 = AXIS2_PLACEMENT_3D ( 'NONE', #2298, #1372, #2024 ) ;
#2906 = PRODUCT_DEFINITION_SHAPE ( 'NONE', 'NONE',  #2220 ) ;
#2907 = EDGE_LOOP ( 'NONE', ( #2342, #945 ) ) ;
#2908 = CARTESIAN_POINT ( 'NONE',  ( -47.49038105676660138, -31.63397459621553054, 6.000000000000000000 ) ) ;
#2909 = AXIS2_PLACEMENT_3D ( 'NONE', #417, #645, #223 ) ;
#2910 = CARTESIAN_POINT ( 'NONE',  ( -59.98076211353318854, -39.99999999999994316, -3.000000000000000888 ) ) ;
#2911 = VECTOR ( 'NONE', #2731, 1000.000000000000114 ) ;
#2912 = ORIENTED_EDGE ( 'NONE', *, *, #1428, .F. ) ;
#2913 = CARTESIAN_POINT ( 'NONE',  ( 0.000000000000000000, 0.000000000000000000, 0.000000000000000000 ) ) ;
#2914 = VERTEX_POINT ( 'NONE', #458 ) ;
#2915 = EDGE_CURVE ( 'NONE', #908, #2070, #857, .T. ) ;
#2916 = EDGE_CURVE ( 'NONE', #2914, #110, #2076, .T. ) ;
#2917 = FACE_OUTER_BOUND ( 'NONE', #1341, .T. ) ;
#2918 = EDGE_CURVE ( 'NONE', #1292, #1462, #512, .T. ) ;
#2919 = EDGE_LOOP ( 'NONE', ( #316, #1269, #2696, #1785 ) ) ;
#2920 = CARTESIAN_POINT ( 'NONE',  ( 6.873863542433761076, -30.00000000000000000, -3.000000000000000000 ) ) ;
#2921 = LINE ( 'NONE', #1767, #829 ) ;
#2922 = ORIENTED_EDGE ( 'NONE', *, *, #495, .T. ) ;
#2923 = EDGE_CURVE ( 'NONE', #339, #1332, #740, .T. ) ;
#2924 = CARTESIAN_POINT ( 'NONE',  ( 6.123233995736766282E-16, -3.999999999999900524, 5.000000000000000000 ) ) ;
#2925 = CARTESIAN_POINT ( 'NONE',  ( 6.123233995736766282E-16, -30.00000000000000000, 5.000000000000000000 ) ) ;
#2926 = ORIENTED_EDGE ( 'NONE', *, *, #971, .F. ) ;
#2927 = LINE ( 'NONE', #1106, #2186 ) ;
#2928 = DIRECTION ( 'NONE',  ( 1.000000000000000000, 0.000000000000000000, 1.076523719386531503E-16 ) ) ;
#2929 = FACE_OUTER_BOUND ( 'NONE', #1479, .T. ) ;
#2930 = ORIENTED_EDGE ( 'NONE', *, *, #2164, .F. ) ;
#2931 = ORIENTED_EDGE ( 'NONE', *, *, #1193, .T. ) ;
#2932 = NEXT_ASSEMBLY_USAGE_OCCURRENCE ( 'NAUO1', ' ', ' ', #2220, #342, $ ) ;
#2933 = NEXT_ASSEMBLY_USAGE_OCCURRENCE ( 'NAUO2', ' ', ' ', #2220, #1107, $ ) ;
#2934 = NEXT_ASSEMBLY_USAGE_OCCURRENCE ( 'NAUO3', ' ', ' ', #2220, #982, $ ) ;
#2935 = NEXT_ASSEMBLY_USAGE_OCCURRENCE ( 'NAUO4', ' ', ' ', #2220, #1387, $ ) ;
#2936=COLOUR_RGB('Dark Blue',0.08,0.2,0.34);
#2937=FILL_AREA_STYLE_COLOUR('',#2936);
#2938=FILL_AREA_STYLE('',(#2937));
#2939=SURFACE_STYLE_FILL_AREA(#2938);
#2940=SURFACE_SIDE_STYLE('',(#2939));
#2941=SURFACE_STYLE_USAGE(.BOTH.,#2940);
#2942=PRESENTATION_STYLE_ASSIGNMENT((#2941));
#2943=COLOUR_RGB('Light Blue',0.38,0.62,0.78);
#2944=FILL_AREA_STYLE_COLOUR('',#2943);
#2945=FILL_AREA_STYLE('',(#2944));
#2946=SURFACE_STYLE_FILL_AREA(#2945);
#2947=SURFACE_SIDE_STYLE('',(#2946));
#2948=SURFACE_STYLE_USAGE(.BOTH.,#2947);
#2949=PRESENTATION_STYLE_ASSIGNMENT((#2948));
#2950=COLOUR_RGB('Sky Blue',0.24,0.69,0.87);
#2951=FILL_AREA_STYLE_COLOUR('',#2950);
#2952=FILL_AREA_STYLE('',(#2951));
#2953=SURFACE_STYLE_FILL_AREA(#2952);
#2954=SURFACE_SIDE_STYLE('',(#2953));
#2955=SURFACE_STYLE_USAGE(.BOTH.,#2954);
#2956=PRESENTATION_STYLE_ASSIGNMENT((#2955));
#2957=COLOUR_RGB('Grey',0.48,0.52,0.57);
#2958=FILL_AREA_STYLE_COLOUR('',#2957);
#2959=FILL_AREA_STYLE('',(#2958));
#2960=SURFACE_STYLE_FILL_AREA(#2959);
#2961=SURFACE_SIDE_STYLE('',(#2960));
#2962=SURFACE_STYLE_USAGE(.BOTH.,#2961);
#2963=PRESENTATION_STYLE_ASSIGNMENT((#2962));
#2964=COLOUR_RGB('Black',0.12,0.14,0.17);
#2965=FILL_AREA_STYLE_COLOUR('',#2964);
#2966=FILL_AREA_STYLE('',(#2965));
#2967=SURFACE_STYLE_FILL_AREA(#2966);
#2968=SURFACE_SIDE_STYLE('',(#2967));
#2969=SURFACE_STYLE_USAGE(.BOTH.,#2968);
#2970=PRESENTATION_STYLE_ASSIGNMENT((#2969));
#2971=COLOUR_RGB('Off White',0.89,0.88,0.83);
#2972=FILL_AREA_STYLE_COLOUR('',#2971);
#2973=FILL_AREA_STYLE('',(#2972));
#2974=SURFACE_STYLE_FILL_AREA(#2973);
#2975=SURFACE_SIDE_STYLE('',(#2974));
#2976=SURFACE_STYLE_USAGE(.BOTH.,#2975);
#2977=PRESENTATION_STYLE_ASSIGNMENT((#2976));
ENDSEC;
END-ISO-10303-21;
